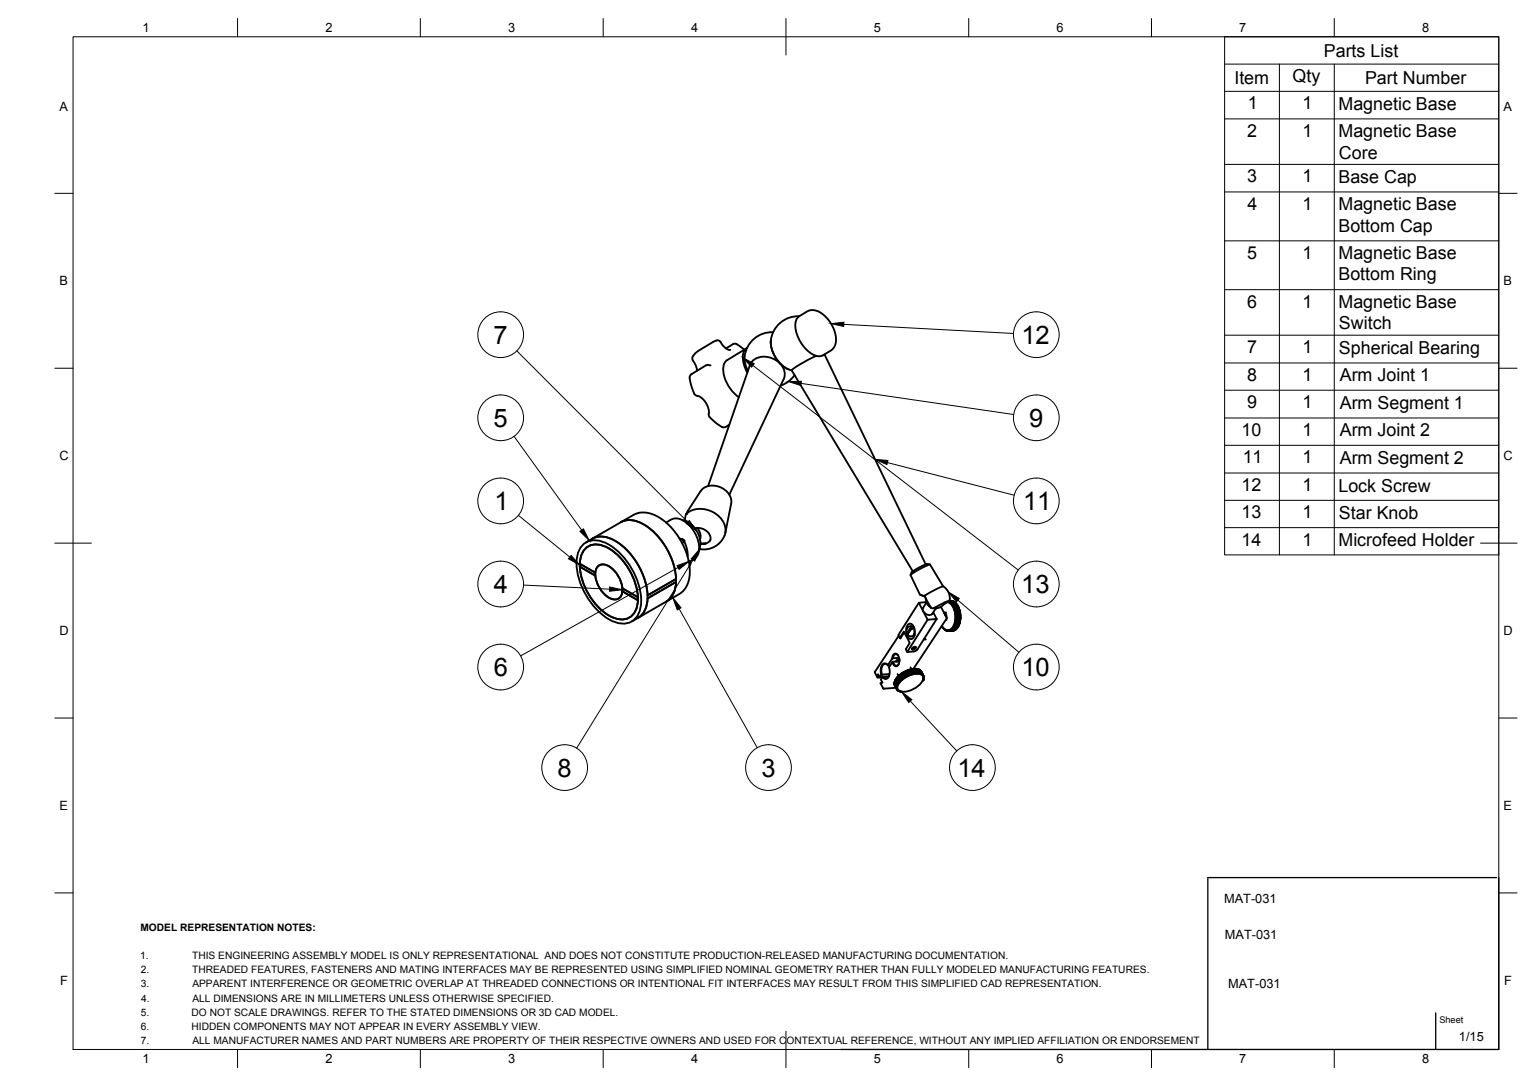
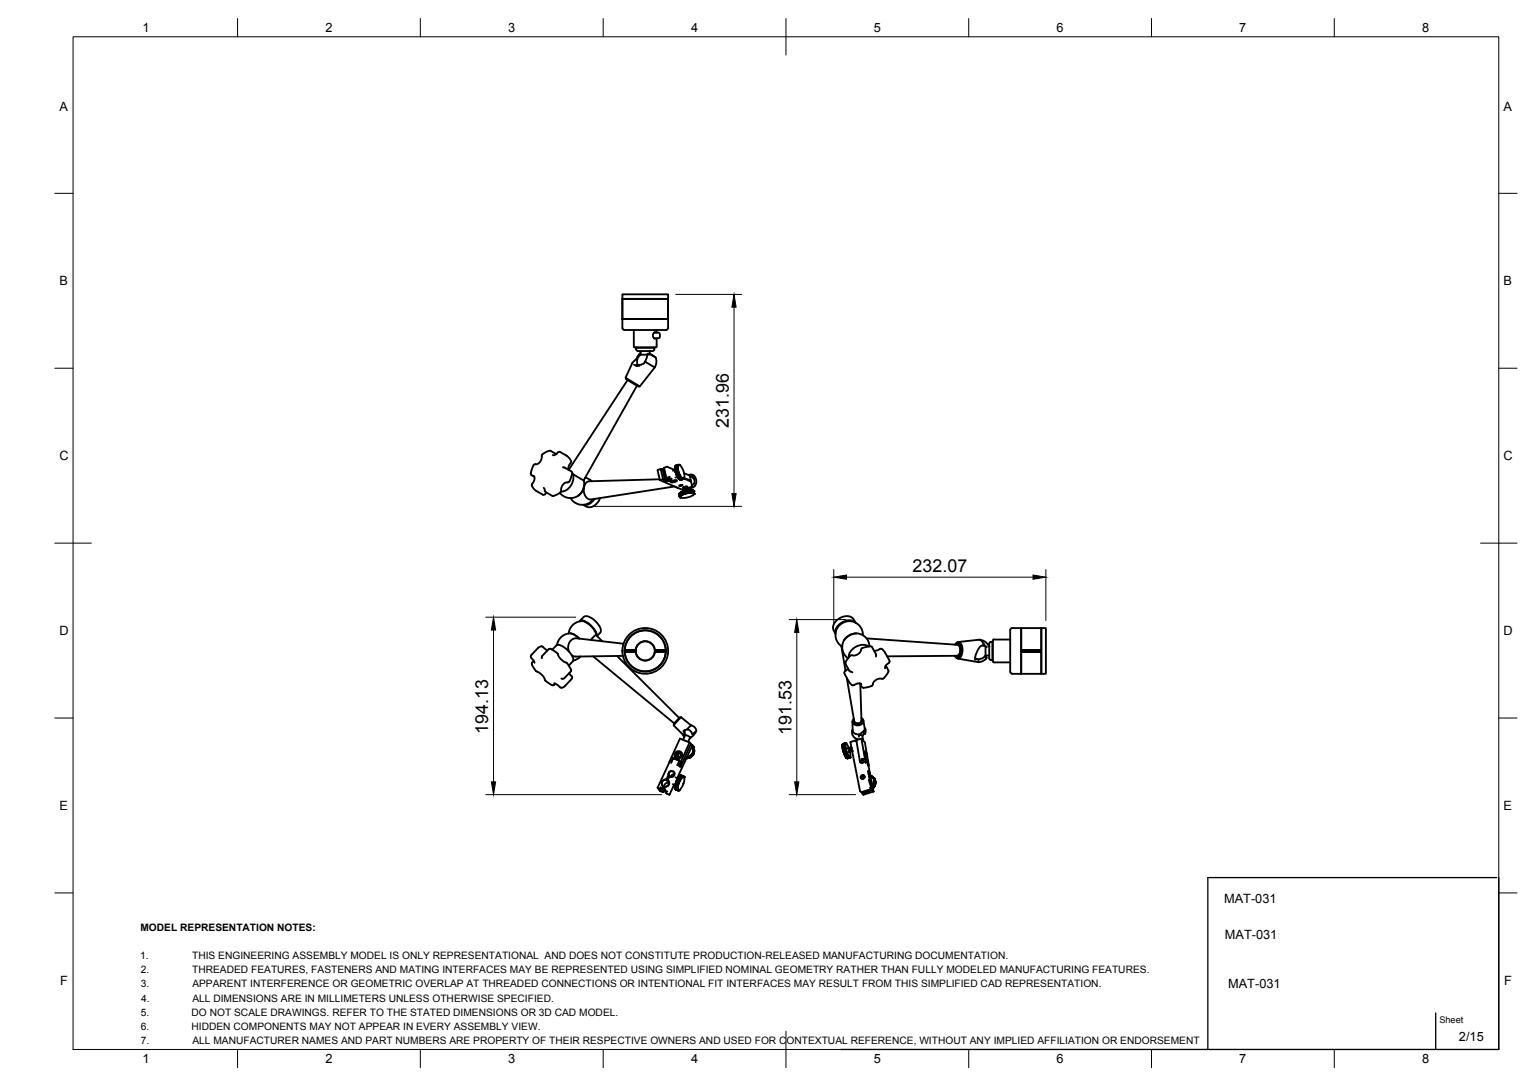
ISO-10303-21;
HEADER;
/* Generated by software containing ST-Developer
 * from STEP Tools, Inc. (www.steptools.com) 
 */

FILE_DESCRIPTION(
/* description */ ('STEP AP214'),
/* implementation_level */ '2;1');

FILE_NAME(
/* name */ 'MAT-031.step',
/* time_stamp */ '2026-11-14T06:58:01-08:00',
/* author */ (''),
/* organization */ (''),
/* preprocessor_version */ 'ST-DEVELOPER v20.2',
/* originating_system */ 'Autodesk Translation Framework v15.17.0.0',
/* authorisation */ '');

FILE_SCHEMA (('AUTOMOTIVE_DESIGN { 1 0 10303 214 3 1 1 }'));
ENDSEC;

DATA;
#10=MECHANICAL_DESIGN_GEOMETRIC_PRESENTATION_REPRESENTATION('',(#1140,#1141,
#1142,#1143,#1144,#1145,#1146,#1147,#1148,#1149,#1150,#1151,#1152,#1153,
#1154,#1155,#1156,#1157,#1158,#1159,#1160,#1161,#1162,#1163,#1164,#1165),
#38635);
#11=ITEM_DEFINED_TRANSFORMATION($,$,#17788,#19729);
#12=ITEM_DEFINED_TRANSFORMATION($,$,#17857,#19730);
#13=ITEM_DEFINED_TRANSFORMATION($,$,#17909,#19731);
#14=ITEM_DEFINED_TRANSFORMATION($,$,#18002,#19732);
#15=ITEM_DEFINED_TRANSFORMATION($,$,#18012,#19733);
#16=ITEM_DEFINED_TRANSFORMATION($,$,#18021,#19734);
#17=ITEM_DEFINED_TRANSFORMATION($,$,#18036,#19735);
#18=ITEM_DEFINED_TRANSFORMATION($,$,#18058,#19736);
#19=ITEM_DEFINED_TRANSFORMATION($,$,#18127,#19737);
#20=ITEM_DEFINED_TRANSFORMATION($,$,#18149,#19738);
#21=ITEM_DEFINED_TRANSFORMATION($,$,#18196,#19739);
#22=ITEM_DEFINED_TRANSFORMATION($,$,#18218,#19740);
#23=ITEM_DEFINED_TRANSFORMATION($,$,#18244,#19741);
#24=ITEM_DEFINED_TRANSFORMATION($,$,#18447,#19742);
#25=(
REPRESENTATION_RELATIONSHIP($,$,#38685,#38684)
REPRESENTATION_RELATIONSHIP_WITH_TRANSFORMATION(#11)
SHAPE_REPRESENTATION_RELATIONSHIP()
);
#26=(
REPRESENTATION_RELATIONSHIP($,$,#38686,#38684)
REPRESENTATION_RELATIONSHIP_WITH_TRANSFORMATION(#12)
SHAPE_REPRESENTATION_RELATIONSHIP()
);
#27=(
REPRESENTATION_RELATIONSHIP($,$,#38687,#38684)
REPRESENTATION_RELATIONSHIP_WITH_TRANSFORMATION(#13)
SHAPE_REPRESENTATION_RELATIONSHIP()
);
#28=(
REPRESENTATION_RELATIONSHIP($,$,#38688,#38684)
REPRESENTATION_RELATIONSHIP_WITH_TRANSFORMATION(#14)
SHAPE_REPRESENTATION_RELATIONSHIP()
);
#29=(
REPRESENTATION_RELATIONSHIP($,$,#38689,#38684)
REPRESENTATION_RELATIONSHIP_WITH_TRANSFORMATION(#15)
SHAPE_REPRESENTATION_RELATIONSHIP()
);
#30=(
REPRESENTATION_RELATIONSHIP($,$,#38690,#38684)
REPRESENTATION_RELATIONSHIP_WITH_TRANSFORMATION(#16)
SHAPE_REPRESENTATION_RELATIONSHIP()
);
#31=(
REPRESENTATION_RELATIONSHIP($,$,#38691,#38684)
REPRESENTATION_RELATIONSHIP_WITH_TRANSFORMATION(#17)
SHAPE_REPRESENTATION_RELATIONSHIP()
);
#32=(
REPRESENTATION_RELATIONSHIP($,$,#38692,#38684)
REPRESENTATION_RELATIONSHIP_WITH_TRANSFORMATION(#18)
SHAPE_REPRESENTATION_RELATIONSHIP()
);
#33=(
REPRESENTATION_RELATIONSHIP($,$,#38693,#38684)
REPRESENTATION_RELATIONSHIP_WITH_TRANSFORMATION(#19)
SHAPE_REPRESENTATION_RELATIONSHIP()
);
#34=(
REPRESENTATION_RELATIONSHIP($,$,#38694,#38684)
REPRESENTATION_RELATIONSHIP_WITH_TRANSFORMATION(#20)
SHAPE_REPRESENTATION_RELATIONSHIP()
);
#35=(
REPRESENTATION_RELATIONSHIP($,$,#38695,#38684)
REPRESENTATION_RELATIONSHIP_WITH_TRANSFORMATION(#21)
SHAPE_REPRESENTATION_RELATIONSHIP()
);
#36=(
REPRESENTATION_RELATIONSHIP($,$,#38696,#38684)
REPRESENTATION_RELATIONSHIP_WITH_TRANSFORMATION(#22)
SHAPE_REPRESENTATION_RELATIONSHIP()
);
#37=(
REPRESENTATION_RELATIONSHIP($,$,#38697,#38684)
REPRESENTATION_RELATIONSHIP_WITH_TRANSFORMATION(#23)
SHAPE_REPRESENTATION_RELATIONSHIP()
);
#38=(
REPRESENTATION_RELATIONSHIP($,$,#38698,#38684)
REPRESENTATION_RELATIONSHIP_WITH_TRANSFORMATION(#24)
SHAPE_REPRESENTATION_RELATIONSHIP()
);
#39=CONTEXT_DEPENDENT_SHAPE_REPRESENTATION(#25,#38670);
#40=CONTEXT_DEPENDENT_SHAPE_REPRESENTATION(#26,#38671);
#41=CONTEXT_DEPENDENT_SHAPE_REPRESENTATION(#27,#38672);
#42=CONTEXT_DEPENDENT_SHAPE_REPRESENTATION(#28,#38673);
#43=CONTEXT_DEPENDENT_SHAPE_REPRESENTATION(#29,#38674);
#44=CONTEXT_DEPENDENT_SHAPE_REPRESENTATION(#30,#38675);
#45=CONTEXT_DEPENDENT_SHAPE_REPRESENTATION(#31,#38676);
#46=CONTEXT_DEPENDENT_SHAPE_REPRESENTATION(#32,#38677);
#47=CONTEXT_DEPENDENT_SHAPE_REPRESENTATION(#33,#38678);
#48=CONTEXT_DEPENDENT_SHAPE_REPRESENTATION(#34,#38679);
#49=CONTEXT_DEPENDENT_SHAPE_REPRESENTATION(#35,#38680);
#50=CONTEXT_DEPENDENT_SHAPE_REPRESENTATION(#36,#38681);
#51=CONTEXT_DEPENDENT_SHAPE_REPRESENTATION(#37,#38682);
#52=CONTEXT_DEPENDENT_SHAPE_REPRESENTATION(#38,#38683);
#53=NEXT_ASSEMBLY_USAGE_OCCURRENCE('Magnetic Base:1','Magnetic Base:1',
'Magnetic Base:1',#38700,#38701,'Magnetic Base:1');
#54=NEXT_ASSEMBLY_USAGE_OCCURRENCE('Magnetic Base Core:1',
'Magnetic Base Core:1','Magnetic Base Core:1',#38700,#38702,
'Magnetic Base Core:1');
#55=NEXT_ASSEMBLY_USAGE_OCCURRENCE('Base Cap:1','Base Cap:1',
'Base Cap:1',#38700,#38703,'Base Cap:1');
#56=NEXT_ASSEMBLY_USAGE_OCCURRENCE('Magnetic Base Bottom Cap:1',
'Magnetic Base Bottom Cap:1','Magnetic Base Bottom Cap:1',#38700,#38704,
'Magnetic Base Bottom Cap:1');
#57=NEXT_ASSEMBLY_USAGE_OCCURRENCE('Magnetic Base Bottom Ring:1',
'Magnetic Base Bottom Ring:1','Magnetic Base Bottom Ring:1',#38700,#38705,
'Magnetic Base Bottom Ring:1');
#58=NEXT_ASSEMBLY_USAGE_OCCURRENCE('Magnetic Base Switch:1',
'Magnetic Base Switch:1','Magnetic Base Switch:1',#38700,#38706,
'Magnetic Base Switch:1');
#59=NEXT_ASSEMBLY_USAGE_OCCURRENCE('Spherical Bearing:1',
'Spherical Bearing:1','Spherical Bearing:1',#38700,#38707,
'Spherical Bearing:1');
#60=NEXT_ASSEMBLY_USAGE_OCCURRENCE('Arm Joint 1:1','Arm Joint 1:1',
'Arm Joint 1:1',#38700,#38708,'Arm Joint 1:1');
#61=NEXT_ASSEMBLY_USAGE_OCCURRENCE('Arm Segment 1:1','Arm Segment 1:1',
'Arm Segment 1:1',#38700,#38709,'Arm Segment 1:1');
#62=NEXT_ASSEMBLY_USAGE_OCCURRENCE('Arm Joint 2:1','Arm Joint 2:1',
'Arm Joint 2:1',#38700,#38710,'Arm Joint 2:1');
#63=NEXT_ASSEMBLY_USAGE_OCCURRENCE('Arm Segment 2:1','Arm Segment 2:1',
'Arm Segment 2:1',#38700,#38711,'Arm Segment 2:1');
#64=NEXT_ASSEMBLY_USAGE_OCCURRENCE('Lock Screw:1','Lock Screw:1',
'Lock Screw:1',#38700,#38712,'Lock Screw:1');
#65=NEXT_ASSEMBLY_USAGE_OCCURRENCE('Star Knob:1','Star Knob:1',
'Star Knob:1',#38700,#38713,'Star Knob:1');
#66=NEXT_ASSEMBLY_USAGE_OCCURRENCE('Microfeed Holder:1',
'Microfeed Holder:1','Microfeed Holder:1',#38700,#38714,
'Microfeed Holder:1');
#67=ELLIPSE('',#18082,0.093043907355238,0.0660721764139862);
#68=ELLIPSE('',#18534,0.424264068711536,0.299999999999714);
#69=ELLIPSE('',#18536,0.424264068712725,0.300000000000503);
#70=ELLIPSE('',#18544,0.424264068711314,0.299999999999553);
#71=ELLIPSE('',#18551,0.424264068712409,0.300000000000364);
#72=ELLIPSE('',#18570,0.424264068711872,0.299999999999922);
#73=ELLIPSE('',#18576,0.42426406871188,0.299999999999951);
#74=ELLIPSE('',#18583,0.424264068709732,0.299999999998459);
#75=ELLIPSE('',#18585,0.424264068710271,0.299999999998872);
#76=ELLIPSE('',#18587,0.424264068711053,0.29999999999941);
#77=ELLIPSE('',#18589,0.424264068710426,0.299999999998988);
#78=SPHERICAL_SURFACE('',#18050,9.);
#79=SPHERICAL_SURFACE('',#18062,1.);
#80=SPHERICAL_SURFACE('',#18074,9.25);
#81=SPHERICAL_SURFACE('',#18083,12.25);
#82=SPHERICAL_SURFACE('',#18107,1.);
#83=SPHERICAL_SURFACE('',#18111,1.);
#84=SPHERICAL_SURFACE('',#18115,1.);
#85=SPHERICAL_SURFACE('',#18118,1.);
#86=SPHERICAL_SURFACE('',#18123,1.);
#87=SPHERICAL_SURFACE('',#18128,15.);
#88=SPHERICAL_SURFACE('',#18136,15.);
#89=SPHERICAL_SURFACE('',#18166,5.5);
#90=SPHERICAL_SURFACE('',#18175,7.70789157434132);
#91=SPHERICAL_SURFACE('',#18197,15.);
#92=SPHERICAL_SURFACE('',#18205,15.);
#93=SPHERICAL_SURFACE('',#18381,2.);
#94=SPHERICAL_SURFACE('',#18383,2.);
#95=SPHERICAL_SURFACE('',#18386,2.);
#96=SPHERICAL_SURFACE('',#18388,2.);
#97=SPHERICAL_SURFACE('',#18394,2.);
#98=SPHERICAL_SURFACE('',#18395,2.);
#99=SPHERICAL_SURFACE('',#18399,2.);
#100=SPHERICAL_SURFACE('',#18400,2.);
#101=SPHERICAL_SURFACE('',#18404,2.);
#102=SPHERICAL_SURFACE('',#18405,2.);
#103=SPHERICAL_SURFACE('',#18409,2.);
#104=SPHERICAL_SURFACE('',#18410,2.);
#105=SPHERICAL_SURFACE('',#18414,2.);
#106=SPHERICAL_SURFACE('',#18416,2.);
#107=SPHERICAL_SURFACE('',#18422,2.);
#108=SPHERICAL_SURFACE('',#18423,2.);
#109=SPHERICAL_SURFACE('',#18424,2.);
#110=SPHERICAL_SURFACE('',#18425,2.);
#111=SPHERICAL_SURFACE('',#18429,2.);
#112=SPHERICAL_SURFACE('',#18431,2.);
#113=SPHERICAL_SURFACE('',#18434,2.);
#114=SPHERICAL_SURFACE('',#18436,2.);
#115=SPHERICAL_SURFACE('',#18442,2.);
#116=SPHERICAL_SURFACE('',#18444,2.);
#117=SPHERICAL_SURFACE('',#18547,0.3);
#118=SPHERICAL_SURFACE('',#18565,0.3);
#119=SPHERICAL_SURFACE('',#18567,0.3);
#120=SPHERICAL_SURFACE('',#18577,0.3);
#121=SPHERICAL_SURFACE('',#18580,0.3);
#122=SPHERICAL_SURFACE('',#18592,0.3);
#123=SPHERICAL_SURFACE('',#18653,5.5);
#124=(
BOUNDED_SURFACE()
B_SPLINE_SURFACE(1,2,((#28370,#28371,#28372,#28373,#28374,#28375,#28376,
#28377,#28378,#28379,#28380,#28381,#28382,#28383,#28384,#28385,#28386,#28387,
#28388,#28389,#28390,#28391,#28392,#28393,#28394,#28395,#28396,#28397,#28398,
#28399,#28400,#28401,#28402,#28403,#28404,#28405,#28406,#28407,#28408,#28409,
#28410,#28411,#28412,#28413,#28414,#28415,#28416,#28417,#28418,#28419,#28420,
#28421,#28422,#28423,#28424,#28425,#28426,#28427,#28428,#28429,#28430,#28431,
#28432,#28433,#28434,#28435,#28436,#28437,#28438,#28439,#28440,#28441,#28442,
#28443,#28444,#28445,#28446,#28447,#28448,#28449,#28450,#28451,#28452,#28453,
#28454,#28455,#28456,#28457,#28458,#28459,#28460,#28461,#28462,#28463,#28464,
#28465,#28466,#28467,#28468,#28469,#28470,#28471,#28472,#28473,#28474,#28475,
#28476,#28477,#28478,#28479,#28480,#28481,#28482,#28483,#28484,#28485,#28486,
#28487,#28488,#28489,#28490,#28491,#28492,#28493,#28494,#28495,#28496,#28497,
#28498,#28499,#28500,#28501,#28502,#28503,#28504,#28505,#28506,#28507,#28508,
#28509,#28510,#28511,#28512,#28513,#28514,#28515,#28516,#28517,#28518,#28519,
#28520,#28521,#28522,#28523,#28524,#28525,#28526,#28527,#28528,#28529,#28530,
#28531,#28532,#28533,#28534,#28535,#28536,#28537,#28538,#28539,#28540,#28541,
#28542,#28543,#28544,#28545,#28546,#28547,#28548,#28549,#28550,#28551,#28552,
#28553,#28554,#28555,#28556,#28557,#28558,#28559,#28560,#28561,#28562,#28563,
#28564,#28565,#28566,#28567,#28568,#28569,#28570,#28571,#28572,#28573,#28574,
#28575,#28576,#28577,#28578,#28579,#28580,#28581,#28582,#28583,#28584,#28585,
#28586,#28587,#28588,#28589,#28590,#28591,#28592,#28593,#28594,#28595,#28596,
#28597,#28598,#28599,#28600,#28601,#28602,#28603,#28604,#28605,#28606,#28607,
#28608,#28609,#28610,#28611,#28612,#28613,#28614,#28615,#28616,#28617,#28618,
#28619,#28620,#28621,#28622,#28623,#28624,#28625,#28626,#28627,#28628,#28629,
#28630,#28631,#28632,#28633,#28634,#28635,#28636,#28637,#28638,#28639,#28640,
#28641,#28642,#28643,#28644,#28645,#28646,#28647,#28648,#28649,#28650,#28651,
#28652,#28653,#28654,#28655,#28656,#28657,#28658,#28659,#28660,#28661,#28662,
#28663,#28664,#28665,#28666,#28667,#28668,#28669,#28670,#28671,#28672,#28673,
#28674,#28675,#28676,#28677,#28678,#28679,#28680,#28681,#28682,#28683,#28684,
#28685,#28686,#28687,#28688,#28689,#28690,#28691,#28692,#28693,#28694,#28695,
#28696,#28697,#28698,#28699,#28700,#28701,#28702,#28703,#28704,#28705,#28706,
#28707,#28708,#28709,#28710,#28711,#28712,#28713,#28714,#28715,#28716,#28717,
#28718,#28719,#28720,#28721,#28722,#28723,#28724,#28725,#28726,#28727,#28728,
#28729,#28730,#28731,#28732,#28733,#28734,#28735,#28736,#28737,#28738,#28739,
#28740,#28741,#28742,#28743,#28744,#28745,#28746,#28747,#28748),(#28749,
#28750,#28751,#28752,#28753,#28754,#28755,#28756,#28757,#28758,#28759,#28760,
#28761,#28762,#28763,#28764,#28765,#28766,#28767,#28768,#28769,#28770,#28771,
#28772,#28773,#28774,#28775,#28776,#28777,#28778,#28779,#28780,#28781,#28782,
#28783,#28784,#28785,#28786,#28787,#28788,#28789,#28790,#28791,#28792,#28793,
#28794,#28795,#28796,#28797,#28798,#28799,#28800,#28801,#28802,#28803,#28804,
#28805,#28806,#28807,#28808,#28809,#28810,#28811,#28812,#28813,#28814,#28815,
#28816,#28817,#28818,#28819,#28820,#28821,#28822,#28823,#28824,#28825,#28826,
#28827,#28828,#28829,#28830,#28831,#28832,#28833,#28834,#28835,#28836,#28837,
#28838,#28839,#28840,#28841,#28842,#28843,#28844,#28845,#28846,#28847,#28848,
#28849,#28850,#28851,#28852,#28853,#28854,#28855,#28856,#28857,#28858,#28859,
#28860,#28861,#28862,#28863,#28864,#28865,#28866,#28867,#28868,#28869,#28870,
#28871,#28872,#28873,#28874,#28875,#28876,#28877,#28878,#28879,#28880,#28881,
#28882,#28883,#28884,#28885,#28886,#28887,#28888,#28889,#28890,#28891,#28892,
#28893,#28894,#28895,#28896,#28897,#28898,#28899,#28900,#28901,#28902,#28903,
#28904,#28905,#28906,#28907,#28908,#28909,#28910,#28911,#28912,#28913,#28914,
#28915,#28916,#28917,#28918,#28919,#28920,#28921,#28922,#28923,#28924,#28925,
#28926,#28927,#28928,#28929,#28930,#28931,#28932,#28933,#28934,#28935,#28936,
#28937,#28938,#28939,#28940,#28941,#28942,#28943,#28944,#28945,#28946,#28947,
#28948,#28949,#28950,#28951,#28952,#28953,#28954,#28955,#28956,#28957,#28958,
#28959,#28960,#28961,#28962,#28963,#28964,#28965,#28966,#28967,#28968,#28969,
#28970,#28971,#28972,#28973,#28974,#28975,#28976,#28977,#28978,#28979,#28980,
#28981,#28982,#28983,#28984,#28985,#28986,#28987,#28988,#28989,#28990,#28991,
#28992,#28993,#28994,#28995,#28996,#28997,#28998,#28999,#29000,#29001,#29002,
#29003,#29004,#29005,#29006,#29007,#29008,#29009,#29010,#29011,#29012,#29013,
#29014,#29015,#29016,#29017,#29018,#29019,#29020,#29021,#29022,#29023,#29024,
#29025,#29026,#29027,#29028,#29029,#29030,#29031,#29032,#29033,#29034,#29035,
#29036,#29037,#29038,#29039,#29040,#29041,#29042,#29043,#29044,#29045,#29046,
#29047,#29048,#29049,#29050,#29051,#29052,#29053,#29054,#29055,#29056,#29057,
#29058,#29059,#29060,#29061,#29062,#29063,#29064,#29065,#29066,#29067,#29068,
#29069,#29070,#29071,#29072,#29073,#29074,#29075,#29076,#29077,#29078,#29079,
#29080,#29081,#29082,#29083,#29084,#29085,#29086,#29087,#29088,#29089,#29090,
#29091,#29092,#29093,#29094,#29095,#29096,#29097,#29098,#29099,#29100,#29101,
#29102,#29103,#29104,#29105,#29106,#29107,#29108,#29109,#29110,#29111,#29112,
#29113,#29114,#29115,#29116,#29117,#29118,#29119,#29120,#29121,#29122,#29123,
#29124,#29125,#29126,#29127)),.UNSPECIFIED.,.F.,.F.,.F.)
B_SPLINE_SURFACE_WITH_KNOTS((2,2),(3,2,2,2,2,2,2,2,2,2,2,2,2,2,2,2,2,2,
2,2,2,2,2,2,2,2,2,2,2,2,2,2,2,2,2,2,2,2,2,2,2,2,2,2,2,2,2,2,2,2,2,2,2,2,
2,2,2,2,2,2,2,2,2,2,2,2,2,2,2,2,2,2,2,2,2,2,2,2,2,2,2,2,2,2,2,2,2,2,2,2,
2,2,2,2,2,2,2,2,2,2,2,2,2,2,2,2,2,2,2,2,2,2,2,2,2,2,2,2,2,2,2,2,2,2,2,2,
2,2,2,2,2,2,2,2,2,2,2,2,2,2,2,2,2,2,2,2,2,2,2,2,2,2,2,2,2,2,2,2,2,2,2,2,
2,2,2,2,2,2,2,2,2,2,2,2,2,2,2,2,2,2,2,2,2,2,2,2,2,2,2,3),(0.,1.),(0.,0.00520833333333333,
0.0104166666666667,0.015625,0.0208333333333333,0.0260416666666667,0.03125,
0.0364583333333333,0.0416666666666667,0.046875,0.0520833333333333,0.0572916666666667,
0.0625,0.0677083333333333,0.0729166666666667,0.078125,0.0833333333333333,
0.0885416666666667,0.09375,0.0989583333333333,0.104166666666667,0.109375,
0.114583333333333,0.119791666666667,0.125,0.130208333333333,0.135416666666667,
0.140625,0.145833333333333,0.151041666666667,0.15625,0.161458333333333,
0.166666666666667,0.171875,0.177083333333333,0.182291666666667,0.1875,0.192708333333333,
0.197916666666667,0.203125,0.208333333333333,0.213541666666667,0.21875,
0.223958333333333,0.229166666666667,0.234375,0.239583333333333,0.244791666666667,
0.25,0.255208333333333,0.260416666666667,0.265625,0.270833333333333,0.276041666666667,
0.28125,0.286458333333333,0.291666666666667,0.296875,0.302083333333333,
0.307291666666667,0.3125,0.317708333333333,0.322916666666667,0.328125,0.333333333333333,
0.338541666666667,0.34375,0.348958333333333,0.354166666666667,0.359375,
0.364583333333333,0.369791666666667,0.375,0.380208333333333,0.385416666666667,
0.390625,0.395833333333333,0.401041666666667,0.40625,0.411458333333333,
0.416666666666667,0.421875,0.427083333333333,0.432291666666667,0.4375,0.442708333333333,
0.447916666666667,0.453125,0.458333333333333,0.463541666666667,0.46875,
0.473958333333333,0.479166666666667,0.484375,0.489583333333333,0.494791666666667,
0.5,0.505208333333333,0.510416666666667,0.515625,0.520833333333333,0.526041666666667,
0.53125,0.536458333333333,0.541666666666667,0.546875,0.552083333333333,
0.557291666666667,0.5625,0.567708333333333,0.572916666666667,0.578125,0.583333333333333,
0.588541666666667,0.59375,0.598958333333333,0.604166666666667,0.609375,
0.614583333333333,0.619791666666667,0.625,0.630208333333333,0.635416666666667,
0.640625,0.645833333333333,0.651041666666667,0.65625,0.661458333333333,
0.666666666666667,0.671875,0.677083333333333,0.682291666666667,0.6875,0.692708333333333,
0.697916666666667,0.703125,0.708333333333333,0.713541666666667,0.71875,
0.723958333333333,0.729166666666667,0.734375,0.739583333333333,0.744791666666667,
0.75,0.755208333333333,0.760416666666667,0.765625,0.770833333333333,0.776041666666667,
0.78125,0.786458333333333,0.791666666666667,0.796875,0.802083333333333,
0.807291666666667,0.8125,0.817708333333333,0.822916666666667,0.828125,0.833333333333333,
0.838541666666667,0.84375,0.848958333333333,0.854166666666667,0.859375,
0.864583333333333,0.869791666666667,0.875,0.880208333333333,0.885416666666667,
0.890625,0.895833333333333,0.901041666666667,0.90625,0.911458333333333,
0.916666666666667,0.921875,0.927083333333333,0.932291666666667,0.9375,0.942708333333333,
0.947916666666667,0.953125,0.958333333333333,0.963541666666667,0.96875,
0.973958333333333,0.979166666666667,0.984246579235552),.UNSPECIFIED.)
GEOMETRIC_REPRESENTATION_ITEM()
RATIONAL_B_SPLINE_SURFACE(((1.,0.866025403784439,1.,0.866025403784439,1.,
0.866025403784439,1.,0.866025403784439,1.,0.866025403784439,1.,0.866025403784439,
1.,0.866025403784439,1.,0.866025403784439,1.,0.866025403784439,1.,0.866025403784439,
1.,0.866025403784439,1.,0.866025403784439,1.,0.866025403784439,1.,0.866025403784439,
1.,0.866025403784439,1.,0.866025403784439,1.,0.866025403784439,1.,0.866025403784439,
1.,0.866025403784439,1.,0.866025403784439,1.,0.866025403784439,1.,0.866025403784439,
1.,0.866025403784439,1.,0.866025403784439,1.,0.866025403784439,1.,0.866025403784439,
1.,0.866025403784439,1.,0.866025403784439,1.,0.866025403784439,1.,0.866025403784439,
1.,0.866025403784439,1.,0.866025403784439,1.,0.866025403784439,1.,0.866025403784439,
1.,0.866025403784439,1.,0.866025403784439,1.,0.866025403784439,1.,0.866025403784439,
1.,0.866025403784439,1.,0.866025403784439,1.,0.866025403784439,1.,0.866025403784439,
1.,0.866025403784439,1.,0.866025403784439,1.,0.866025403784439,1.,0.866025403784439,
1.,0.866025403784439,1.,0.866025403784439,1.,0.866025403784439,1.,0.866025403784439,
1.,0.866025403784439,1.,0.866025403784439,1.,0.866025403784439,1.,0.866025403784439,
1.,0.866025403784439,1.,0.866025403784439,1.,0.866025403784439,1.,0.866025403784439,
1.,0.866025403784439,1.,0.866025403784439,1.,0.866025403784439,1.,0.866025403784439,
1.,0.866025403784439,1.,0.866025403784439,1.,0.866025403784439,1.,0.866025403784439,
1.,0.866025403784439,1.,0.866025403784439,1.,0.866025403784439,1.,0.866025403784439,
1.,0.866025403784439,1.,0.866025403784439,1.,0.866025403784439,1.,0.866025403784439,
1.,0.866025403784439,1.,0.866025403784439,1.,0.866025403784439,1.,0.866025403784439,
1.,0.866025403784439,1.,0.866025403784439,1.,0.866025403784439,1.,0.866025403784439,
1.,0.866025403784439,1.,0.866025403784439,1.,0.866025403784439,1.,0.866025403784439,
1.,0.866025403784439,1.,0.866025403784439,1.,0.866025403784439,1.,0.866025403784439,
1.,0.866025403784439,1.,0.866025403784439,1.,0.866025403784439,1.,0.866025403784439,
1.,0.866025403784439,1.,0.866025403784439,1.,0.866025403784439,1.,0.866025403784439,
1.,0.866025403784439,1.,0.866025403784439,1.,0.866025403784439,1.,0.866025403784439,
1.,0.866025403784439,1.,0.866025403784439,1.,0.866025403784439,1.,0.866025403784439,
1.,0.866025403784439,1.,0.866025403784439,1.,0.866025403784439,1.,0.866025403784439,
1.,0.866025403784439,1.,0.866025403784439,1.,0.866025403784439,1.,0.866025403784439,
1.,0.866025403784439,1.,0.866025403784439,1.,0.866025403784439,1.,0.866025403784439,
1.,0.866025403784439,1.,0.866025403784439,1.,0.866025403784439,1.,0.866025403784439,
1.,0.866025403784439,1.,0.866025403784439,1.,0.866025403784439,1.,0.866025403784439,
1.,0.866025403784439,1.,0.866025403784439,1.,0.866025403784439,1.,0.866025403784439,
1.,0.866025403784439,1.,0.866025403784439,1.,0.866025403784439,1.,0.866025403784439,
1.,0.866025403784439,1.,0.866025403784439,1.,0.866025403784439,1.,0.866025403784439,
1.,0.866025403784439,1.,0.866025403784439,1.,0.866025403784439,1.,0.866025403784439,
1.,0.866025403784439,1.,0.866025403784439,1.,0.866025403784439,1.,0.866025403784439,
1.,0.866025403784439,1.,0.866025403784439,1.,0.866025403784439,1.,0.866025403784439,
1.,0.866025403784439,1.,0.866025403784439,1.,0.866025403784439,1.,0.866025403784439,
1.,0.866025403784439,1.,0.866025403784439,1.,0.866025403784439,1.,0.866025403784439,
1.,0.866025403784439,1.,0.866025403784439,1.,0.866025403784439,1.,0.866025403784439,
1.,0.866025403784439,1.,0.866025403784439,1.,0.866025403784439,1.,0.866025403784439,
1.,0.866025403784439,1.,0.866025403784439,1.,0.866025403784439,1.,0.866025403784439,
1.,0.866025403784439,1.,0.866025403784439,1.,0.866025403784439,1.,0.866025403784439,
1.,0.866025403784439,1.,0.866025403784439,1.,0.866025403784439,1.,0.866025403784439,
1.,0.866025403784439,1.,0.866025403784439,1.,0.866025403784439,1.,0.866025403784439,
1.,0.866025403784439,1.,0.866025403784439,1.,0.866025403784439,1.,0.866025403784439,
1.,0.866025403784439,1.,0.866025403784439,1.,0.869328786836457,0.993556135519056),
(1.,0.866025403784439,1.,0.866025403784439,1.,0.866025403784439,1.,0.866025403784439,
1.,0.866025403784439,1.,0.866025403784439,1.,0.866025403784439,1.,0.866025403784439,
1.,0.866025403784439,1.,0.866025403784439,1.,0.866025403784439,1.,0.866025403784439,
1.,0.866025403784439,1.,0.866025403784439,1.,0.866025403784439,1.,0.866025403784439,
1.,0.866025403784439,1.,0.866025403784439,1.,0.866025403784439,1.,0.866025403784439,
1.,0.866025403784439,1.,0.866025403784439,1.,0.866025403784439,1.,0.866025403784439,
1.,0.866025403784439,1.,0.866025403784439,1.,0.866025403784439,1.,0.866025403784439,
1.,0.866025403784439,1.,0.866025403784439,1.,0.866025403784439,1.,0.866025403784439,
1.,0.866025403784439,1.,0.866025403784439,1.,0.866025403784439,1.,0.866025403784439,
1.,0.866025403784439,1.,0.866025403784439,1.,0.866025403784439,1.,0.866025403784439,
1.,0.866025403784439,1.,0.866025403784439,1.,0.866025403784439,1.,0.866025403784439,
1.,0.866025403784439,1.,0.866025403784439,1.,0.866025403784439,1.,0.866025403784439,
1.,0.866025403784439,1.,0.866025403784439,1.,0.866025403784439,1.,0.866025403784439,
1.,0.866025403784439,1.,0.866025403784439,1.,0.866025403784439,1.,0.866025403784439,
1.,0.866025403784439,1.,0.866025403784439,1.,0.866025403784439,1.,0.866025403784439,
1.,0.866025403784439,1.,0.866025403784439,1.,0.866025403784439,1.,0.866025403784439,
1.,0.866025403784439,1.,0.866025403784439,1.,0.866025403784439,1.,0.866025403784439,
1.,0.866025403784439,1.,0.866025403784439,1.,0.866025403784439,1.,0.866025403784439,
1.,0.866025403784439,1.,0.866025403784439,1.,0.866025403784439,1.,0.866025403784439,
1.,0.866025403784439,1.,0.866025403784439,1.,0.866025403784439,1.,0.866025403784439,
1.,0.866025403784439,1.,0.866025403784439,1.,0.866025403784439,1.,0.866025403784439,
1.,0.866025403784439,1.,0.866025403784439,1.,0.866025403784439,1.,0.866025403784439,
1.,0.866025403784439,1.,0.866025403784439,1.,0.866025403784439,1.,0.866025403784439,
1.,0.866025403784439,1.,0.866025403784439,1.,0.866025403784439,1.,0.866025403784439,
1.,0.866025403784439,1.,0.866025403784439,1.,0.866025403784439,1.,0.866025403784439,
1.,0.866025403784439,1.,0.866025403784439,1.,0.866025403784439,1.,0.866025403784439,
1.,0.866025403784439,1.,0.866025403784439,1.,0.866025403784439,1.,0.866025403784439,
1.,0.866025403784439,1.,0.866025403784439,1.,0.866025403784439,1.,0.866025403784439,
1.,0.866025403784439,1.,0.866025403784439,1.,0.866025403784439,1.,0.866025403784439,
1.,0.866025403784439,1.,0.866025403784439,1.,0.866025403784439,1.,0.866025403784439,
1.,0.866025403784439,1.,0.866025403784439,1.,0.866025403784439,1.,0.866025403784439,
1.,0.866025403784439,1.,0.866025403784439,1.,0.866025403784439,1.,0.866025403784439,
1.,0.866025403784439,1.,0.866025403784439,1.,0.866025403784439,1.,0.866025403784439,
1.,0.866025403784439,1.,0.866025403784439,1.,0.866025403784439,1.,0.866025403784439,
1.,0.866025403784439,1.,0.866025403784439,1.,0.866025403784439,1.,0.866025403784439,
1.,0.866025403784439,1.,0.866025403784439,1.,0.866025403784439,1.,0.866025403784439,
1.,0.866025403784439,1.,0.866025403784439,1.,0.866025403784439,1.,0.866025403784439,
1.,0.866025403784439,1.,0.866025403784439,1.,0.866025403784439,1.,0.866025403784439,
1.,0.866025403784439,1.,0.866025403784439,1.,0.866025403784439,1.,0.866025403784439,
1.,0.866025403784439,1.,0.866025403784439,1.,0.866025403784439,1.,0.866025403784439,
1.,0.866025403784439,1.,0.866025403784439,1.,0.866025403784439,1.,0.866025403784439,
1.,0.866025403784439,1.,0.866025403784439,1.,0.866025403784439,1.,0.866025403784439,
1.,0.866025403784439,1.,0.866025403784439,1.,0.866025403784439,1.,0.866025403784439,
1.,0.866025403784439,1.,0.866025403784439,1.,0.866025403784439,1.,0.866025403784439,
1.,0.866025403784439,1.,0.866025403784439,1.,0.866025403784439,1.,0.866025403784439,
1.,0.866025403784439,1.,0.866025403784439,1.,0.866025403784439,1.,0.866025403784439,
1.,0.866025403784439,1.,0.866025403784439,1.,0.866025403784439,1.,0.866025403784439,
1.,0.869328786836457,0.993556135519056)))
REPRESENTATION_ITEM('')
SURFACE()
);
#125=(
BOUNDED_SURFACE()
B_SPLINE_SURFACE(1,2,((#29128,#29129,#29130,#29131,#29132,#29133,#29134,
#29135,#29136,#29137,#29138,#29139,#29140,#29141,#29142,#29143,#29144,#29145,
#29146,#29147,#29148,#29149,#29150,#29151,#29152,#29153,#29154,#29155,#29156,
#29157,#29158,#29159,#29160,#29161,#29162,#29163,#29164,#29165,#29166,#29167,
#29168,#29169,#29170,#29171,#29172,#29173,#29174,#29175,#29176,#29177,#29178,
#29179,#29180,#29181,#29182,#29183,#29184,#29185,#29186,#29187,#29188,#29189,
#29190,#29191,#29192,#29193,#29194,#29195,#29196,#29197,#29198,#29199,#29200,
#29201,#29202,#29203,#29204,#29205,#29206,#29207,#29208,#29209,#29210,#29211,
#29212,#29213,#29214,#29215,#29216,#29217,#29218,#29219,#29220,#29221,#29222,
#29223,#29224,#29225,#29226,#29227,#29228,#29229,#29230,#29231,#29232,#29233,
#29234,#29235,#29236,#29237,#29238,#29239,#29240,#29241,#29242,#29243,#29244,
#29245,#29246,#29247,#29248,#29249,#29250,#29251,#29252,#29253,#29254,#29255,
#29256,#29257,#29258,#29259,#29260,#29261,#29262,#29263,#29264,#29265,#29266,
#29267,#29268,#29269,#29270,#29271,#29272,#29273,#29274,#29275,#29276,#29277,
#29278,#29279,#29280,#29281,#29282,#29283,#29284,#29285,#29286,#29287,#29288,
#29289,#29290,#29291,#29292,#29293,#29294,#29295,#29296,#29297,#29298,#29299,
#29300,#29301,#29302,#29303,#29304,#29305,#29306,#29307,#29308,#29309,#29310,
#29311,#29312,#29313,#29314,#29315,#29316,#29317,#29318,#29319,#29320,#29321,
#29322,#29323,#29324,#29325,#29326,#29327,#29328,#29329,#29330,#29331,#29332,
#29333,#29334,#29335,#29336,#29337,#29338,#29339,#29340,#29341,#29342,#29343,
#29344,#29345,#29346,#29347,#29348,#29349,#29350,#29351,#29352,#29353,#29354,
#29355,#29356,#29357,#29358,#29359,#29360,#29361,#29362,#29363,#29364,#29365,
#29366,#29367,#29368,#29369,#29370,#29371,#29372,#29373,#29374,#29375,#29376,
#29377,#29378,#29379,#29380,#29381,#29382,#29383,#29384,#29385,#29386,#29387,
#29388,#29389,#29390,#29391,#29392,#29393,#29394,#29395,#29396,#29397,#29398,
#29399,#29400,#29401,#29402,#29403,#29404,#29405,#29406,#29407,#29408,#29409,
#29410,#29411,#29412,#29413,#29414,#29415,#29416,#29417,#29418,#29419,#29420,
#29421,#29422,#29423,#29424,#29425,#29426,#29427,#29428,#29429,#29430,#29431,
#29432,#29433,#29434,#29435,#29436,#29437,#29438,#29439,#29440,#29441,#29442,
#29443,#29444,#29445,#29446,#29447,#29448,#29449,#29450,#29451,#29452,#29453,
#29454,#29455,#29456,#29457,#29458,#29459,#29460,#29461,#29462,#29463,#29464,
#29465,#29466,#29467,#29468,#29469,#29470,#29471,#29472,#29473,#29474,#29475,
#29476,#29477,#29478,#29479,#29480,#29481,#29482,#29483,#29484,#29485,#29486,
#29487,#29488,#29489,#29490,#29491,#29492,#29493,#29494,#29495,#29496,#29497,
#29498,#29499,#29500,#29501,#29502,#29503,#29504,#29505,#29506),(#29507,
#29508,#29509,#29510,#29511,#29512,#29513,#29514,#29515,#29516,#29517,#29518,
#29519,#29520,#29521,#29522,#29523,#29524,#29525,#29526,#29527,#29528,#29529,
#29530,#29531,#29532,#29533,#29534,#29535,#29536,#29537,#29538,#29539,#29540,
#29541,#29542,#29543,#29544,#29545,#29546,#29547,#29548,#29549,#29550,#29551,
#29552,#29553,#29554,#29555,#29556,#29557,#29558,#29559,#29560,#29561,#29562,
#29563,#29564,#29565,#29566,#29567,#29568,#29569,#29570,#29571,#29572,#29573,
#29574,#29575,#29576,#29577,#29578,#29579,#29580,#29581,#29582,#29583,#29584,
#29585,#29586,#29587,#29588,#29589,#29590,#29591,#29592,#29593,#29594,#29595,
#29596,#29597,#29598,#29599,#29600,#29601,#29602,#29603,#29604,#29605,#29606,
#29607,#29608,#29609,#29610,#29611,#29612,#29613,#29614,#29615,#29616,#29617,
#29618,#29619,#29620,#29621,#29622,#29623,#29624,#29625,#29626,#29627,#29628,
#29629,#29630,#29631,#29632,#29633,#29634,#29635,#29636,#29637,#29638,#29639,
#29640,#29641,#29642,#29643,#29644,#29645,#29646,#29647,#29648,#29649,#29650,
#29651,#29652,#29653,#29654,#29655,#29656,#29657,#29658,#29659,#29660,#29661,
#29662,#29663,#29664,#29665,#29666,#29667,#29668,#29669,#29670,#29671,#29672,
#29673,#29674,#29675,#29676,#29677,#29678,#29679,#29680,#29681,#29682,#29683,
#29684,#29685,#29686,#29687,#29688,#29689,#29690,#29691,#29692,#29693,#29694,
#29695,#29696,#29697,#29698,#29699,#29700,#29701,#29702,#29703,#29704,#29705,
#29706,#29707,#29708,#29709,#29710,#29711,#29712,#29713,#29714,#29715,#29716,
#29717,#29718,#29719,#29720,#29721,#29722,#29723,#29724,#29725,#29726,#29727,
#29728,#29729,#29730,#29731,#29732,#29733,#29734,#29735,#29736,#29737,#29738,
#29739,#29740,#29741,#29742,#29743,#29744,#29745,#29746,#29747,#29748,#29749,
#29750,#29751,#29752,#29753,#29754,#29755,#29756,#29757,#29758,#29759,#29760,
#29761,#29762,#29763,#29764,#29765,#29766,#29767,#29768,#29769,#29770,#29771,
#29772,#29773,#29774,#29775,#29776,#29777,#29778,#29779,#29780,#29781,#29782,
#29783,#29784,#29785,#29786,#29787,#29788,#29789,#29790,#29791,#29792,#29793,
#29794,#29795,#29796,#29797,#29798,#29799,#29800,#29801,#29802,#29803,#29804,
#29805,#29806,#29807,#29808,#29809,#29810,#29811,#29812,#29813,#29814,#29815,
#29816,#29817,#29818,#29819,#29820,#29821,#29822,#29823,#29824,#29825,#29826,
#29827,#29828,#29829,#29830,#29831,#29832,#29833,#29834,#29835,#29836,#29837,
#29838,#29839,#29840,#29841,#29842,#29843,#29844,#29845,#29846,#29847,#29848,
#29849,#29850,#29851,#29852,#29853,#29854,#29855,#29856,#29857,#29858,#29859,
#29860,#29861,#29862,#29863,#29864,#29865,#29866,#29867,#29868,#29869,#29870,
#29871,#29872,#29873,#29874,#29875,#29876,#29877,#29878,#29879,#29880,#29881,
#29882,#29883,#29884,#29885)),.UNSPECIFIED.,.F.,.F.,.F.)
B_SPLINE_SURFACE_WITH_KNOTS((2,2),(3,2,2,2,2,2,2,2,2,2,2,2,2,2,2,2,2,2,
2,2,2,2,2,2,2,2,2,2,2,2,2,2,2,2,2,2,2,2,2,2,2,2,2,2,2,2,2,2,2,2,2,2,2,2,
2,2,2,2,2,2,2,2,2,2,2,2,2,2,2,2,2,2,2,2,2,2,2,2,2,2,2,2,2,2,2,2,2,2,2,2,
2,2,2,2,2,2,2,2,2,2,2,2,2,2,2,2,2,2,2,2,2,2,2,2,2,2,2,2,2,2,2,2,2,2,2,2,
2,2,2,2,2,2,2,2,2,2,2,2,2,2,2,2,2,2,2,2,2,2,2,2,2,2,2,2,2,2,2,2,2,2,2,2,
2,2,2,2,2,2,2,2,2,2,2,2,2,2,2,2,2,2,2,2,2,2,2,2,2,2,2,3),(0.,1.),(0.,0.00520833333333333,
0.0104166666666667,0.015625,0.0208333333333333,0.0260416666666667,0.03125,
0.0364583333333333,0.0416666666666667,0.046875,0.0520833333333333,0.0572916666666667,
0.0625,0.0677083333333333,0.0729166666666667,0.078125,0.0833333333333333,
0.0885416666666667,0.09375,0.0989583333333333,0.104166666666667,0.109375,
0.114583333333333,0.119791666666667,0.125,0.130208333333333,0.135416666666667,
0.140625,0.145833333333333,0.151041666666667,0.15625,0.161458333333333,
0.166666666666667,0.171875,0.177083333333333,0.182291666666667,0.1875,0.192708333333333,
0.197916666666667,0.203125,0.208333333333333,0.213541666666667,0.21875,
0.223958333333333,0.229166666666667,0.234375,0.239583333333333,0.244791666666667,
0.25,0.255208333333333,0.260416666666667,0.265625,0.270833333333333,0.276041666666667,
0.28125,0.286458333333333,0.291666666666667,0.296875,0.302083333333333,
0.307291666666667,0.3125,0.317708333333333,0.322916666666667,0.328125,0.333333333333333,
0.338541666666667,0.34375,0.348958333333333,0.354166666666667,0.359375,
0.364583333333333,0.369791666666667,0.375,0.380208333333333,0.385416666666667,
0.390625,0.395833333333333,0.401041666666667,0.40625,0.411458333333333,
0.416666666666667,0.421875,0.427083333333333,0.432291666666667,0.4375,0.442708333333333,
0.447916666666667,0.453125,0.458333333333333,0.463541666666667,0.46875,
0.473958333333333,0.479166666666667,0.484375,0.489583333333333,0.494791666666667,
0.5,0.505208333333333,0.510416666666667,0.515625,0.520833333333333,0.526041666666667,
0.53125,0.536458333333333,0.541666666666667,0.546875,0.552083333333333,
0.557291666666667,0.5625,0.567708333333333,0.572916666666667,0.578125,0.583333333333333,
0.588541666666667,0.59375,0.598958333333333,0.604166666666667,0.609375,
0.614583333333333,0.619791666666667,0.625,0.630208333333333,0.635416666666667,
0.640625,0.645833333333333,0.651041666666667,0.65625,0.661458333333333,
0.666666666666667,0.671875,0.677083333333333,0.682291666666667,0.6875,0.692708333333333,
0.697916666666667,0.703125,0.708333333333333,0.713541666666667,0.71875,
0.723958333333333,0.729166666666667,0.734375,0.739583333333333,0.744791666666667,
0.75,0.755208333333333,0.760416666666667,0.765625,0.770833333333333,0.776041666666667,
0.78125,0.786458333333333,0.791666666666667,0.796875,0.802083333333333,
0.807291666666667,0.8125,0.817708333333333,0.822916666666667,0.828125,0.833333333333333,
0.838541666666667,0.84375,0.848958333333333,0.854166666666667,0.859375,
0.864583333333333,0.869791666666667,0.875,0.880208333333333,0.885416666666667,
0.890625,0.895833333333333,0.901041666666667,0.90625,0.911458333333333,
0.916666666666667,0.921875,0.927083333333333,0.932291666666667,0.9375,0.942708333333333,
0.947916666666667,0.953125,0.958333333333333,0.963541666666667,0.96875,
0.973958333333333,0.979166666666667,0.984246579355594),.UNSPECIFIED.)
GEOMETRIC_REPRESENTATION_ITEM()
RATIONAL_B_SPLINE_SURFACE(((1.,0.866025403784439,1.,0.866025403784439,1.,
0.866025403784439,1.,0.866025403784439,1.,0.866025403784439,1.,0.866025403784439,
1.,0.866025403784439,1.,0.866025403784439,1.,0.866025403784439,1.,0.866025403784439,
1.,0.866025403784439,1.,0.866025403784439,1.,0.866025403784439,1.,0.866025403784439,
1.,0.866025403784439,1.,0.866025403784439,1.,0.866025403784439,1.,0.866025403784439,
1.,0.866025403784439,1.,0.866025403784439,1.,0.866025403784439,1.,0.866025403784439,
1.,0.866025403784439,1.,0.866025403784439,1.,0.866025403784439,1.,0.866025403784439,
1.,0.866025403784439,1.,0.866025403784439,1.,0.866025403784439,1.,0.866025403784439,
1.,0.866025403784439,1.,0.866025403784439,1.,0.866025403784439,1.,0.866025403784439,
1.,0.866025403784439,1.,0.866025403784439,1.,0.866025403784439,1.,0.866025403784439,
1.,0.866025403784439,1.,0.866025403784439,1.,0.866025403784439,1.,0.866025403784439,
1.,0.866025403784439,1.,0.866025403784439,1.,0.866025403784439,1.,0.866025403784439,
1.,0.866025403784439,1.,0.866025403784439,1.,0.866025403784439,1.,0.866025403784439,
1.,0.866025403784439,1.,0.866025403784439,1.,0.866025403784439,1.,0.866025403784439,
1.,0.866025403784439,1.,0.866025403784439,1.,0.866025403784439,1.,0.866025403784439,
1.,0.866025403784439,1.,0.866025403784439,1.,0.866025403784439,1.,0.866025403784439,
1.,0.866025403784439,1.,0.866025403784439,1.,0.866025403784439,1.,0.866025403784439,
1.,0.866025403784439,1.,0.866025403784439,1.,0.866025403784439,1.,0.866025403784439,
1.,0.866025403784439,1.,0.866025403784439,1.,0.866025403784439,1.,0.866025403784439,
1.,0.866025403784439,1.,0.866025403784439,1.,0.866025403784439,1.,0.866025403784439,
1.,0.866025403784439,1.,0.866025403784439,1.,0.866025403784439,1.,0.866025403784439,
1.,0.866025403784439,1.,0.866025403784439,1.,0.866025403784439,1.,0.866025403784439,
1.,0.866025403784439,1.,0.866025403784439,1.,0.866025403784439,1.,0.866025403784439,
1.,0.866025403784439,1.,0.866025403784439,1.,0.866025403784439,1.,0.866025403784439,
1.,0.866025403784439,1.,0.866025403784439,1.,0.866025403784439,1.,0.866025403784439,
1.,0.866025403784439,1.,0.866025403784439,1.,0.866025403784439,1.,0.866025403784439,
1.,0.866025403784439,1.,0.866025403784439,1.,0.866025403784439,1.,0.866025403784439,
1.,0.866025403784439,1.,0.866025403784439,1.,0.866025403784439,1.,0.866025403784439,
1.,0.866025403784439,1.,0.866025403784439,1.,0.866025403784439,1.,0.866025403784439,
1.,0.866025403784439,1.,0.866025403784439,1.,0.866025403784439,1.,0.866025403784439,
1.,0.866025403784439,1.,0.866025403784439,1.,0.866025403784439,1.,0.866025403784439,
1.,0.866025403784439,1.,0.866025403784439,1.,0.866025403784439,1.,0.866025403784439,
1.,0.866025403784439,1.,0.866025403784439,1.,0.866025403784439,1.,0.866025403784439,
1.,0.866025403784439,1.,0.866025403784439,1.,0.866025403784439,1.,0.866025403784439,
1.,0.866025403784439,1.,0.866025403784439,1.,0.866025403784439,1.,0.866025403784439,
1.,0.866025403784439,1.,0.866025403784439,1.,0.866025403784439,1.,0.866025403784439,
1.,0.866025403784439,1.,0.866025403784439,1.,0.866025403784439,1.,0.866025403784439,
1.,0.866025403784439,1.,0.866025403784439,1.,0.866025403784439,1.,0.866025403784439,
1.,0.866025403784439,1.,0.866025403784439,1.,0.866025403784439,1.,0.866025403784439,
1.,0.866025403784439,1.,0.866025403784439,1.,0.866025403784439,1.,0.866025403784439,
1.,0.866025403784439,1.,0.866025403784439,1.,0.866025403784439,1.,0.866025403784439,
1.,0.866025403784439,1.,0.866025403784439,1.,0.866025403784439,1.,0.866025403784439,
1.,0.866025403784439,1.,0.866025403784439,1.,0.866025403784439,1.,0.866025403784439,
1.,0.866025403784439,1.,0.866025403784439,1.,0.866025403784439,1.,0.866025403784439,
1.,0.866025403784439,1.,0.866025403784439,1.,0.866025403784439,1.,0.866025403784439,
1.,0.866025403784439,1.,0.866025403784439,1.,0.866025403784439,1.,0.866025403784439,
1.,0.866025403784439,1.,0.866025403784439,1.,0.866025403784439,1.,0.866025403784439,
1.,0.866025403784439,1.,0.866025403784439,1.,0.869328783748594,0.993556141390235),
(1.,0.866025403784439,1.,0.866025403784439,1.,0.866025403784439,1.,0.866025403784439,
1.,0.866025403784439,1.,0.866025403784439,1.,0.866025403784439,1.,0.866025403784439,
1.,0.866025403784439,1.,0.866025403784439,1.,0.866025403784439,1.,0.866025403784439,
1.,0.866025403784439,1.,0.866025403784439,1.,0.866025403784439,1.,0.866025403784439,
1.,0.866025403784439,1.,0.866025403784439,1.,0.866025403784439,1.,0.866025403784439,
1.,0.866025403784439,1.,0.866025403784439,1.,0.866025403784439,1.,0.866025403784439,
1.,0.866025403784439,1.,0.866025403784439,1.,0.866025403784439,1.,0.866025403784439,
1.,0.866025403784439,1.,0.866025403784439,1.,0.866025403784439,1.,0.866025403784439,
1.,0.866025403784439,1.,0.866025403784439,1.,0.866025403784439,1.,0.866025403784439,
1.,0.866025403784439,1.,0.866025403784439,1.,0.866025403784439,1.,0.866025403784439,
1.,0.866025403784439,1.,0.866025403784439,1.,0.866025403784439,1.,0.866025403784439,
1.,0.866025403784439,1.,0.866025403784439,1.,0.866025403784439,1.,0.866025403784439,
1.,0.866025403784439,1.,0.866025403784439,1.,0.866025403784439,1.,0.866025403784439,
1.,0.866025403784439,1.,0.866025403784439,1.,0.866025403784439,1.,0.866025403784439,
1.,0.866025403784439,1.,0.866025403784439,1.,0.866025403784439,1.,0.866025403784439,
1.,0.866025403784439,1.,0.866025403784439,1.,0.866025403784439,1.,0.866025403784439,
1.,0.866025403784439,1.,0.866025403784439,1.,0.866025403784439,1.,0.866025403784439,
1.,0.866025403784439,1.,0.866025403784439,1.,0.866025403784439,1.,0.866025403784439,
1.,0.866025403784439,1.,0.866025403784439,1.,0.866025403784439,1.,0.866025403784439,
1.,0.866025403784439,1.,0.866025403784439,1.,0.866025403784439,1.,0.866025403784439,
1.,0.866025403784439,1.,0.866025403784439,1.,0.866025403784439,1.,0.866025403784439,
1.,0.866025403784439,1.,0.866025403784439,1.,0.866025403784439,1.,0.866025403784439,
1.,0.866025403784439,1.,0.866025403784439,1.,0.866025403784439,1.,0.866025403784439,
1.,0.866025403784439,1.,0.866025403784439,1.,0.866025403784439,1.,0.866025403784439,
1.,0.866025403784439,1.,0.866025403784439,1.,0.866025403784439,1.,0.866025403784439,
1.,0.866025403784439,1.,0.866025403784439,1.,0.866025403784439,1.,0.866025403784439,
1.,0.866025403784439,1.,0.866025403784439,1.,0.866025403784439,1.,0.866025403784439,
1.,0.866025403784439,1.,0.866025403784439,1.,0.866025403784439,1.,0.866025403784439,
1.,0.866025403784439,1.,0.866025403784439,1.,0.866025403784439,1.,0.866025403784439,
1.,0.866025403784439,1.,0.866025403784439,1.,0.866025403784439,1.,0.866025403784439,
1.,0.866025403784439,1.,0.866025403784439,1.,0.866025403784439,1.,0.866025403784439,
1.,0.866025403784439,1.,0.866025403784439,1.,0.866025403784439,1.,0.866025403784439,
1.,0.866025403784439,1.,0.866025403784439,1.,0.866025403784439,1.,0.866025403784439,
1.,0.866025403784439,1.,0.866025403784439,1.,0.866025403784439,1.,0.866025403784439,
1.,0.866025403784439,1.,0.866025403784439,1.,0.866025403784439,1.,0.866025403784439,
1.,0.866025403784439,1.,0.866025403784439,1.,0.866025403784439,1.,0.866025403784439,
1.,0.866025403784439,1.,0.866025403784439,1.,0.866025403784439,1.,0.866025403784439,
1.,0.866025403784439,1.,0.866025403784439,1.,0.866025403784439,1.,0.866025403784439,
1.,0.866025403784439,1.,0.866025403784439,1.,0.866025403784439,1.,0.866025403784439,
1.,0.866025403784439,1.,0.866025403784439,1.,0.866025403784439,1.,0.866025403784439,
1.,0.866025403784439,1.,0.866025403784439,1.,0.866025403784439,1.,0.866025403784439,
1.,0.866025403784439,1.,0.866025403784439,1.,0.866025403784439,1.,0.866025403784439,
1.,0.866025403784439,1.,0.866025403784439,1.,0.866025403784439,1.,0.866025403784439,
1.,0.866025403784439,1.,0.866025403784439,1.,0.866025403784439,1.,0.866025403784439,
1.,0.866025403784439,1.,0.866025403784439,1.,0.866025403784439,1.,0.866025403784439,
1.,0.866025403784439,1.,0.866025403784439,1.,0.866025403784439,1.,0.866025403784439,
1.,0.866025403784439,1.,0.866025403784439,1.,0.866025403784439,1.,0.866025403784439,
1.,0.869328783748594,0.993556141390235)))
REPRESENTATION_ITEM('')
SURFACE()
);
#126=(
BOUNDED_SURFACE()
B_SPLINE_SURFACE(3,2,((#31255,#31256,#31257),(#31258,#31259,#31260),(#31261,
#31262,#31263),(#31264,#31265,#31266),(#31267,#31268,#31269),(#31270,#31271,
#31272),(#31273,#31274,#31275),(#31276,#31277,#31278),(#31279,#31280,#31281),
(#31282,#31283,#31284),(#31285,#31286,#31287),(#31288,#31289,#31290),(#31291,
#31292,#31293),(#31294,#31295,#31296),(#31297,#31298,#31299),(#31300,#31301,
#31302),(#31303,#31304,#31305),(#31306,#31307,#31308),(#31309,#31310,#31311),
(#31312,#31313,#31314),(#31315,#31316,#31317),(#31318,#31319,#31320),(#31321,
#31322,#31323),(#31324,#31325,#31326)),.UNSPECIFIED.,.F.,.F.,.F.)
B_SPLINE_SURFACE_WITH_KNOTS((4,2,2,2,2,2,2,2,2,2,2,4),(3,3),(-4.33680868994202E-19,
0.00199566610229966,0.00299349915344949,0.00399133220459933,0.00598699830689899,
0.00698483135804882,0.00748374788362374,0.00773320614641119,0.00785793527780492,
0.00792029984350179,0.00795148212635022,0.00798266440919865),(-8.88988013967173,
1.),.UNSPECIFIED.)
GEOMETRIC_REPRESENTATION_ITEM()
RATIONAL_B_SPLINE_SURFACE(((1.03673130903543,0.997934094247711,1.),(1.03429323702968,
0.998071220506301,1.),(1.03166096458261,0.99821926932168,1.),(1.02743039620336,
0.998457212258636,1.),(1.0259730109093,0.99853918104062,1.),(1.02296180766651,
0.998708542336582,1.),(1.02140250811888,0.998796243156116,1.),(1.01667872310722,
0.999061926435161,1.),(1.0134397522586,0.999244098230379,1.),(1.00845036900139,
0.999524719744889,1.),(1.00676184803489,0.99961968845875,1.),(1.00420736775411,
0.999763361952692,1.),(1.00335516609469,0.999811292950975,1.),(1.00207805691192,
0.999883122332401,1.),(1.00165222462761,0.999907072727549,1.),(1.00101619611475,
0.999942845342188,1.),(1.000804914933,0.999954728583493,1.),(1.00049166224454,
0.99997234708248,1.),(1.00038777606523,0.999978190028486,1.),(1.00023475952815,
0.999986796248967,1.),(1.00018401486096,0.999989650318224,1.),(1.00008917562832,
0.999994984430222,1.),(1.00003836348216,0.999997842294746,1.),(1.00003093298314,
0.999998260213712,1.)))
REPRESENTATION_ITEM('')
SURFACE()
);
#127=(
BOUNDED_SURFACE()
B_SPLINE_SURFACE(3,2,((#31328,#31329,#31330),(#31331,#31332,#31333),(#31334,
#31335,#31336),(#31337,#31338,#31339),(#31340,#31341,#31342),(#31343,#31344,
#31345),(#31346,#31347,#31348),(#31349,#31350,#31351),(#31352,#31353,#31354),
(#31355,#31356,#31357),(#31358,#31359,#31360),(#31361,#31362,#31363),(#31364,
#31365,#31366),(#31367,#31368,#31369),(#31370,#31371,#31372),(#31373,#31374,
#31375)),.UNSPECIFIED.,.F.,.F.,.F.)
B_SPLINE_SURFACE_WITH_KNOTS((4,2,2,2,2,2,2,4),(3,3),(-1.37073647788269E-16,
3.79857431933033E-5,7.59714863867437E-5,0.000151942972773624,0.000303885945547386,
0.000607771891094909,0.00121554378218996,0.00243108756438005),(-0.000101005518536674,
1.),.UNSPECIFIED.)
GEOMETRIC_REPRESENTATION_ITEM()
RATIONAL_B_SPLINE_SURFACE(((1.00000004220253,0.999791088022201,1.),(1.00000004430103,
0.999780699959677,1.),(1.00000006201562,0.999693008760642,1.),(1.00000010657676,
0.999472421084997,1.),(1.00000013303073,0.999341468019306,1.),(1.00000021861,
0.998917831394663,1.),(1.00000028470715,0.998590635693005,1.),(1.00000049900653,
0.997529805625635,1.),(1.00000066545063,0.996705869955465,1.),(1.00000123037801,
0.993909352546599,1.),(1.00000169504325,0.99160915523887,1.),(1.00000335151631,
0.983409241593269,1.),(1.00000480674396,0.976205537946754,1.),(1.00001025390194,
0.949240882635747,1.),(1.00001533088998,0.924108651696566,1.),(1.00002191434951,
0.891519048541741,1.)))
REPRESENTATION_ITEM('')
SURFACE()
);
#128=(
BOUNDED_SURFACE()
B_SPLINE_SURFACE(3,2,((#31377,#31378,#31379),(#31380,#31381,#31382),(#31383,
#31384,#31385),(#31386,#31387,#31388)),.UNSPECIFIED.,.F.,.F.,.F.)
B_SPLINE_SURFACE_WITH_KNOTS((4,4),(3,3),(-1.3918214625889E-5,0.00121512868205196),
(0.,1.00001391821463),.UNSPECIFIED.)
GEOMETRIC_REPRESENTATION_ITEM()
RATIONAL_B_SPLINE_SURFACE(((0.999999999999999,0.891779221283223,1.00000301248005),
(1.,0.884413245314419,1.00000321752252),(1.,0.87579683831728,1.00000345737252),
(1.,0.866200683852581,1.0000037244952)))
REPRESENTATION_ITEM('')
SURFACE()
);
#129=(
BOUNDED_SURFACE()
B_SPLINE_SURFACE(3,2,((#31400,#31401,#31402),(#31403,#31404,#31405),(#31406,
#31407,#31408),(#31409,#31410,#31411),(#31412,#31413,#31414),(#31415,#31416,
#31417),(#31418,#31419,#31420),(#31421,#31422,#31423),(#31424,#31425,#31426),
(#31427,#31428,#31429),(#31430,#31431,#31432),(#31433,#31434,#31435),(#31436,
#31437,#31438),(#31439,#31440,#31441)),.UNSPECIFIED.,.F.,.F.,.F.)
B_SPLINE_SURFACE_WITH_KNOTS((4,2,2,2,2,2,4),(3,3),(0.033103384374427,0.0355583288461946,
0.0367823574217915,0.0380063859973883,0.0392304145729851,0.0404544431485819,
0.0429025002997755),(0.,1.00000688732057),.UNSPECIFIED.)
GEOMETRIC_REPRESENTATION_ITEM()
RATIONAL_B_SPLINE_SURFACE(((1.,0.211850238456311,1.00001085648014),(1.,
0.211789774891773,1.000010857313),(1.,0.211720587176297,1.00001085826604),
(1.,0.21160403471626,1.0000108598715),(1.,0.211562868788471,1.00001086043855),
(1.,0.211477187752812,1.00001086161878),(1.,0.211433005503744,1.00001086222737),
(1.,0.211342033825223,1.00001086348047),(1.,0.211295244231205,1.00001086412498),
(1.,0.211199020809361,1.00001086545043),(1.,0.211149240972151,1.00001086613613),
(1.,0.21099910955097,1.00001086820413),(1.,0.210897693883658,1.0000108696011),
(1.,0.21079496787879,1.00001087101611)))
REPRESENTATION_ITEM('')
SURFACE()
);
#130=(
BOUNDED_SURFACE()
B_SPLINE_SURFACE(3,2,((#31518,#31519,#31520),(#31521,#31522,#31523),(#31524,
#31525,#31526),(#31527,#31528,#31529),(#31530,#31531,#31532),(#31533,#31534,
#31535),(#31536,#31537,#31538),(#31539,#31540,#31541),(#31542,#31543,#31544),
(#31545,#31546,#31547),(#31548,#31549,#31550),(#31551,#31552,#31553),(#31554,
#31555,#31556),(#31557,#31558,#31559),(#31560,#31561,#31562),(#31563,#31564,
#31565),(#31566,#31567,#31568),(#31569,#31570,#31571),(#31572,#31573,#31574),
(#31575,#31576,#31577),(#31578,#31579,#31580),(#31581,#31582,#31583),(#31584,
#31585,#31586),(#31587,#31588,#31589),(#31590,#31591,#31592),(#31593,#31594,
#31595),(#31596,#31597,#31598),(#31599,#31600,#31601),(#31602,#31603,#31604),
(#31605,#31606,#31607),(#31608,#31609,#31610),(#31611,#31612,#31613),(#31614,
#31615,#31616),(#31617,#31618,#31619),(#31620,#31621,#31622),(#31623,#31624,
#31625),(#31626,#31627,#31628),(#31629,#31630,#31631),(#31632,#31633,#31634),
(#31635,#31636,#31637),(#31638,#31639,#31640),(#31641,#31642,#31643),(#31644,
#31645,#31646),(#31647,#31648,#31649),(#31650,#31651,#31652),(#31653,#31654,
#31655),(#31656,#31657,#31658),(#31659,#31660,#31661),(#31662,#31663,#31664),
(#31665,#31666,#31667),(#31668,#31669,#31670),(#31671,#31672,#31673),(#31674,
#31675,#31676),(#31677,#31678,#31679),(#31680,#31681,#31682),(#31683,#31684,
#31685),(#31686,#31687,#31688),(#31689,#31690,#31691),(#31692,#31693,#31694),
(#31695,#31696,#31697),(#31698,#31699,#31700),(#31701,#31702,#31703),(#31704,
#31705,#31706),(#31707,#31708,#31709),(#31710,#31711,#31712),(#31713,#31714,
#31715),(#31716,#31717,#31718),(#31719,#31720,#31721),(#31722,#31723,#31724),
(#31725,#31726,#31727),(#31728,#31729,#31730),(#31731,#31732,#31733),(#31734,
#31735,#31736),(#31737,#31738,#31739),(#31740,#31741,#31742),(#31743,#31744,
#31745)),.UNSPECIFIED.,.F.,.F.,.F.)
B_SPLINE_SURFACE_WITH_KNOTS((4,2,2,2,2,2,2,2,2,2,2,2,2,2,2,2,2,2,2,2,2,
2,2,2,2,2,2,2,2,2,2,2,2,2,2,2,2,4),(3,3),(0.0155469420440516,0.0160999385621218,
0.016652935080192,0.0172059315982622,0.0177589281163324,0.0183119246344026,
0.0188649211524727,0.0194179176705429,0.0199709141886131,0.0210769072247535,
0.0221829002608939,0.0232888932970342,0.0243948863331746,0.025500879369315,
0.0266068724054554,0.0288188584777361,0.0299248515138765,0.0310308445500169,
0.0321368375861573,0.0332428306222976,0.034348823658438,0.0354548166945784,
0.0376668027668591,0.0398787888391399,0.0409847818752803,0.0420907749114206,
0.043196767947561,0.0443027609837014,0.0454087540198418,0.0465147470559821,
0.0470677435740523,0.0476207400921225,0.0481737366101927,0.0487267331282629,
0.0492797296463331,0.0498327261644033,0.0503857226824734,0.0509387192005436),
(0.,1.),.UNSPECIFIED.)
GEOMETRIC_REPRESENTATION_ITEM()
RATIONAL_B_SPLINE_SURFACE(((1.,0.229526735048257,1.),(1.,0.224133558219702,
1.),(1.,0.219259724176961,1.),(1.,0.211064181475465,1.),(1.,0.207811801710184,
1.),(1.,0.203341888285831,1.),(1.,0.202127973482812,1.),(1.,0.201960202180378,
1.),(1.,0.203032258888432,1.),(1.,0.207289559269388,1.),(1.,0.210454353335156,
1.),(1.,0.218450587215706,1.),(1.,0.223279069424003,1.),(1.,0.234195834429115,
1.),(1.,0.240233471751073,1.),(1.,0.252998923243242,1.),(1.,0.259742761586636,
1.),(1.,0.28067947683831,1.),(1.,0.295554256169214,1.),(1.,0.326016231928046,
1.),(1.,0.341634062441765,1.),(1.,0.372564100762139,1.),(1.,0.387951242324607,
1.),(1.,0.418305222299702,1.),(1.,0.433275214730199,1.),(1.,0.46261806682354,
1.),(1.,0.476992506609391,1.),(1.,0.504978264480088,1.),(1.,0.518645722843901,
1.),(1.,0.557478084599559,1.),(1.,0.580701256089758,1.),(1.,0.610367709572221,
1.),(1.,0.619422302565764,1.),(1.,0.635083430287347,1.),(1.,0.64175221457835,
1.),(1.,0.65261413861016,1.),(1.,0.656808227795975,1.),(1.,0.662484548907152,
1.),(1.,0.663913234852522,1.),(1.,0.663922009369197,1.),(1.,0.66252245378572,
1.),(1.,0.656942975295251,1.),(1.,0.652711192029527,1.),(1.,0.636300872830255,
1.),(1.,0.620465569188766,1.),(1.,0.580610974593483,1.),(1.,0.557339096866905,
1.),(1.,0.518721884857682,1.),(1.,0.505222106533921,1.),(1.,0.477115614134931,
1.),(1.,0.462576289466857,1.),(1.,0.433080321145928,1.),(1.,0.418066573341961,
1.),(1.,0.387696762864547,1.),(1.,0.372337606905373,1.),(1.,0.341539686788467,
1.),(1.,0.326093173961657,1.),(1.,0.295606321651459,1.),(1.,0.280553638483726,
1.),(1.,0.25953297193159,1.),(1.,0.252774217996814,1.),(1.,0.240006731870622,
1.),(1.,0.233989040402757,1.),(1.,0.223104380065769,1.),(1.,0.218299068913211,
1.),(1.,0.210355245717533,1.),(1.,0.207219723680965,1.),(1.,0.203010941824996,
1.),(1.,0.201948260378419,1.),(1.,0.202143131871967,1.),(1.,0.203375531025685,
1.),(1.,0.207855714464755,1.),(1.,0.211099729925129,1.),(1.,0.219230361697907,
1.),(1.,0.224140752438636,1.),(1.,0.229539201120578,1.)))
REPRESENTATION_ITEM('')
SURFACE()
);
#131=(
BOUNDED_SURFACE()
B_SPLINE_SURFACE(3,2,((#31822,#31823,#31824),(#31825,#31826,#31827),(#31828,
#31829,#31830),(#31831,#31832,#31833),(#31834,#31835,#31836),(#31837,#31838,
#31839),(#31840,#31841,#31842),(#31843,#31844,#31845),(#31846,#31847,#31848),
(#31849,#31850,#31851),(#31852,#31853,#31854),(#31855,#31856,#31857),(#31858,
#31859,#31860),(#31861,#31862,#31863)),.UNSPECIFIED.,.F.,.F.,.F.)
B_SPLINE_SURFACE_WITH_KNOTS((4,2,2,2,2,2,4),(3,3),(0.0331033843745195,0.0355583288461946,
0.0367823574217914,0.0380063859973882,0.039230414572985,0.0404544431485818,
0.0429025002997754),(-6.88732048148063E-6,1.),.UNSPECIFIED.)
GEOMETRIC_REPRESENTATION_ITEM()
RATIONAL_B_SPLINE_SURFACE(((1.00001085647999,0.211850238456374,0.999999999999999),
(1.00001085731285,0.211789774892188,1.),(1.00001085826589,0.211720587175911,
1.),(1.00001085987136,0.211604034716559,1.),(1.0000108604384,0.211562868788407,
1.),(1.00001086161863,0.211477187753023,1.),(1.00001086222722,0.211433005503953,
1.),(1.00001086348033,0.21134203382516,1.),(1.00001086412484,0.211295244231278,
1.),(1.00001086545028,0.211199020809434,1.),(1.00001086613598,0.211149240972224,
1.),(1.00001086820399,0.210999109551043,1.),(1.00001086960095,0.21089769388373,
1.),(1.00001087101596,0.210794967878863,1.)))
REPRESENTATION_ITEM('')
SURFACE()
);
#132=(
BOUNDED_SURFACE()
B_SPLINE_SURFACE(3,2,((#31872,#31873,#31874),(#31875,#31876,#31877),(#31878,
#31879,#31880),(#31881,#31882,#31883)),.UNSPECIFIED.,.F.,.F.,.F.)
B_SPLINE_SURFACE_WITH_KNOTS((4,4),(3,3),(-1.39182146545714E-5,0.00121512868208074),
(0.,1.00001391821465),.UNSPECIFIED.)
GEOMETRIC_REPRESENTATION_ITEM()
RATIONAL_B_SPLINE_SURFACE(((1.,0.866200683851906,1.00000372449521),(1.,
0.875796838317096,1.00000345737253),(1.,0.884413245314652,1.00000321752253),
(1.,0.891779221283738,1.00000301248006)))
REPRESENTATION_ITEM('')
SURFACE()
);
#133=(
BOUNDED_SURFACE()
B_SPLINE_SURFACE(3,2,((#31885,#31886,#31887),(#31888,#31889,#31890),(#31891,
#31892,#31893),(#31894,#31895,#31896),(#31897,#31898,#31899),(#31900,#31901,
#31902),(#31903,#31904,#31905),(#31906,#31907,#31908),(#31909,#31910,#31911),
(#31912,#31913,#31914),(#31915,#31916,#31917),(#31918,#31919,#31920),(#31921,
#31922,#31923),(#31924,#31925,#31926)),.UNSPECIFIED.,.F.,.F.,.F.)
B_SPLINE_SURFACE_WITH_KNOTS((4,2,2,2,2,2,4),(3,3),(-0.000142750203022182,
0.00120936219001056,0.00181404328501584,0.00211638383251848,0.0022675541062698,
0.00234313924314546,0.0025614745830495),(-0.00757884796103774,1.),
 .UNSPECIFIED.)
GEOMETRIC_REPRESENTATION_ITEM()
RATIONAL_B_SPLINE_SURFACE(((1.00183804612443,0.878738422126962,1.),(1.00124990939078,
0.917539618342774,1.),(1.00080710421406,0.946752843030485,1.),(1.00036309214798,
0.976045689935564,1.),(1.00025309503348,0.983302539200046,1.),(1.00012791013031,
0.991561373775666,1.),(1.00009280627034,0.993877283802622,1.),(1.00005012171262,
0.996693315865673,1.),(1.00003753469437,0.997523720322227,1.),(1.00002137280872,
0.998589969819041,1.),(1.00001641874054,0.998916804993093,1.),(0.999999713951067,
1.00001887153131,1.),(0.999989596975289,1.00068631965997,1.),(1.00005723328726,
0.996224143329086,0.999999999999999)))
REPRESENTATION_ITEM('')
SURFACE()
);
#134=(
BOUNDED_SURFACE()
B_SPLINE_SURFACE(3,2,((#31928,#31929,#31930),(#31931,#31932,#31933),(#31934,
#31935,#31936),(#31937,#31938,#31939),(#31940,#31941,#31942),(#31943,#31944,
#31945),(#31946,#31947,#31948),(#31949,#31950,#31951),(#31952,#31953,#31954),
(#31955,#31956,#31957),(#31958,#31959,#31960),(#31961,#31962,#31963),(#31964,
#31965,#31966),(#31967,#31968,#31969),(#31970,#31971,#31972),(#31973,#31974,
#31975),(#31976,#31977,#31978),(#31979,#31980,#31981),(#31982,#31983,#31984),
(#31985,#31986,#31987),(#31988,#31989,#31990),(#31991,#31992,#31993),(#31994,
#31995,#31996),(#31997,#31998,#31999)),.UNSPECIFIED.,.F.,.F.,.F.)
B_SPLINE_SURFACE_WITH_KNOTS((4,2,2,2,2,2,2,2,2,2,2,4),(3,3),(0.,0.00199566610230272,
0.00299349915345408,0.00399133220460544,0.00598699830690816,0.00698483135805952,
0.0074837478836352,0.00773320614642304,0.00785793527781696,0.00792029984351392,
0.0079514821263624,0.00798266440921088),(0.,9.4347309660509),
 .UNSPECIFIED.)
GEOMETRIC_REPRESENTATION_ITEM()
RATIONAL_B_SPLINE_SURFACE(((1.,0.998029170758512,1.03324682886395),(1.,
0.99815998623251,1.03104004220522),(1.,0.998301221588568,1.02865747774274),
(1.,0.998528213985216,1.02482823814861),(1.,0.99860641042422,1.0235091062976),
(1.,0.998767977423409,1.0207835579553),(1.,0.998851642101808,1.01937217984798),
(1.,0.999105098182627,1.01509651214116),(1.,0.999278886120722,1.01216480313518),
(1.,0.999546592953898,1.00764873290395),(1.,0.999637191045363,1.00612039184888),
(1.,0.999774252439753,1.00380823987384),(1.,0.999819977571642,1.00303688150212),
(1.,0.999888501242266,1.00188092404907),(1.,0.999911349399373,1.00149548793254),
(1.,0.99994547569713,1.00091979565164),(1.,0.999956812051398,1.00072855745488),
(1.,0.999973619716972,1.0004450211803),(1.,0.999979193760625,1.00035099006309),
(1.,0.999987403908142,1.0002124892921),(1.,0.999990126628257,1.00016655846877),
(1.,0.999995215255311,1.00008071606839),(1.,0.999997941596032,1.00003472416737),
(1.,0.999998340281648,1.00002799855556)))
REPRESENTATION_ITEM('')
SURFACE()
);
#135=(
BOUNDED_SURFACE()
B_SPLINE_SURFACE(3,2,((#32683,#32684,#32685),(#32686,#32687,#32688),(#32689,
#32690,#32691),(#32692,#32693,#32694),(#32695,#32696,#32697),(#32698,#32699,
#32700),(#32701,#32702,#32703),(#32704,#32705,#32706),(#32707,#32708,#32709),
(#32710,#32711,#32712),(#32713,#32714,#32715),(#32716,#32717,#32718),(#32719,
#32720,#32721),(#32722,#32723,#32724),(#32725,#32726,#32727),(#32728,#32729,
#32730),(#32731,#32732,#32733),(#32734,#32735,#32736),(#32737,#32738,#32739),
(#32740,#32741,#32742),(#32743,#32744,#32745),(#32746,#32747,#32748)),
 .UNSPECIFIED.,.F.,.F.,.F.)
B_SPLINE_SURFACE_WITH_KNOTS((4,2,2,2,2,2,2,2,2,2,4),(3,3),(0.00881272913566369,
0.00928844068390005,0.00953838644963798,0.00978833221537591,0.0100382779811138,
0.0105381695125897,0.0110380610440656,0.0120378441070173,0.0125377356384932,
0.0127876814042311,0.01326339295247),(-0.00102566064560791,1.),
 .UNSPECIFIED.)
GEOMETRIC_REPRESENTATION_ITEM()
RATIONAL_B_SPLINE_SURFACE(((1.00132329066919,0.354908139032077,1.),(1.00124812393843,
0.391551219315617,1.),(1.00115915858371,0.434921000104149,1.),(1.00102358876472,
0.501010022609669,1.),(1.00097653790903,0.523946875988812,1.),(1.00088693501083,
0.567627453274935,1.),(1.00084389129738,0.588610862181495,1.),(1.00076096626522,
0.629036042047148,1.),(1.00072089412048,0.648570838919578,1.),(1.00060683104295,
0.704175525527758,1.),(1.00053863758583,0.737419199938388,1.),(1.00041471240488,
0.797831569997033,1.),(1.00035895931741,0.825010680216488,1.),(1.00021007792585,
0.897588970214807,1.),(1.00013587466058,0.933762370057051,1.),(1.00006032673641,
0.970591278572527,1.),(1.00004117816685,0.979926027666627,1.),(1.00002165568508,
0.989443055473061,1.),(1.00001667885161,0.991869215376876,1.),(1.00000682799133,
0.99667141789903,1.),(1.00000607453102,0.997038722775045,1.),(1.00001271218793,
0.993802926931325,1.)))
REPRESENTATION_ITEM('')
SURFACE()
);
#136=(
BOUNDED_SURFACE()
B_SPLINE_SURFACE(3,2,((#32822,#32823,#32824),(#32825,#32826,#32827),(#32828,
#32829,#32830),(#32831,#32832,#32833),(#32834,#32835,#32836),(#32837,#32838,
#32839),(#32840,#32841,#32842),(#32843,#32844,#32845),(#32846,#32847,#32848),
(#32849,#32850,#32851),(#32852,#32853,#32854),(#32855,#32856,#32857),(#32858,
#32859,#32860),(#32861,#32862,#32863),(#32864,#32865,#32866),(#32867,#32868,
#32869),(#32870,#32871,#32872),(#32873,#32874,#32875),(#32876,#32877,#32878),
(#32879,#32880,#32881),(#32882,#32883,#32884),(#32885,#32886,#32887),(#32888,
#32889,#32890),(#32891,#32892,#32893),(#32894,#32895,#32896),(#32897,#32898,
#32899),(#32900,#32901,#32902),(#32903,#32904,#32905)),.UNSPECIFIED.,.F.,
 .F.,.F.)
B_SPLINE_SURFACE_WITH_KNOTS((4,2,2,2,2,2,2,2,2,2,2,2,2,4),(3,3),(0.0120978781599544,
0.013608206651586,0.0151185351432177,0.0158736993890335,0.0166288636348494,
0.0173840278806652,0.018139192126481,0.0188943563722969,0.0196495206181127,
0.0204046848639285,0.0211598491097444,0.0219150133555602,0.022670177601376,
0.0241805060930077),(0.,1.00005676629322),.UNSPECIFIED.)
GEOMETRIC_REPRESENTATION_ITEM()
RATIONAL_B_SPLINE_SURFACE(((1.,0.419714375858336,1.00006588132778),(1.,
0.455258548961405,1.00006184590587),(1.,0.490259453324333,1.00005787216267),
(1.,0.554227398223351,1.00005060971644),(1.,0.583234396585999,1.00004731647689),
(1.,0.620852932125695,1.00004304554726),(1.,0.632335513594305,1.00004174190008),
(1.,0.652343207191375,1.00003947037488),(1.,0.660962788243787,1.00003849177155),
(1.,0.67512712292899,1.000036883658),(1.,0.680682058163542,1.00003625299183),
(1.,0.688032273240624,1.0000354185029),(1.,0.689900381447712,1.00003520641175),
(1.,0.689947597716664,1.00003520105116),(1.,0.688072411855674,1.00003541394586),
(1.,0.680752669873931,1.0000362449751),(1.,0.675339625853613,1.00003685953199),
(1.,0.661242565913974,1.00003846000767),(1.,0.652474855221301,1.00003945542854),
(1.,0.632370855573539,1.00004173788762),(1.,0.621020695612542,1.00004302650063),
(1.,0.596023875522447,1.00004586445427),(1.,0.582284387510476,1.00004742433388),
(1.,0.553320360279571,1.00005071269481),(1.,0.538073094759082,1.0000524437563),
(1.,0.490378194191559,1.00005785868172),(1.,0.455940368475232,1.00006176849714),
(1.,0.419656970284633,1.00006588784518)))
REPRESENTATION_ITEM('')
SURFACE()
);
#137=(
BOUNDED_SURFACE()
B_SPLINE_SURFACE(3,2,((#32908,#32909,#32910),(#32911,#32912,#32913),(#32914,
#32915,#32916),(#32917,#32918,#32919),(#32920,#32921,#32922),(#32923,#32924,
#32925),(#32926,#32927,#32928),(#32929,#32930,#32931),(#32932,#32933,#32934),
(#32935,#32936,#32937),(#32938,#32939,#32940),(#32941,#32942,#32943),(#32944,
#32945,#32946),(#32947,#32948,#32949),(#32950,#32951,#32952),(#32953,#32954,
#32955),(#32956,#32957,#32958),(#32959,#32960,#32961),(#32962,#32963,#32964),
(#32965,#32966,#32967),(#32968,#32969,#32970),(#32971,#32972,#32973)),
 .UNSPECIFIED.,.F.,.F.,.F.)
B_SPLINE_SURFACE_WITH_KNOTS((4,2,2,2,2,2,2,2,2,2,4),(3,3),(0.0086385816929815,
0.00928844068390017,0.00953838644963812,0.00978833221537607,0.010038277981114,
0.0105381695125899,0.0110380610440658,0.0120378441070176,0.0125377356384935,
0.0127876814042315,0.0134375403951501),(0.,1.00153795011474),
 .UNSPECIFIED.)
GEOMETRIC_REPRESENTATION_ITEM()
RATIONAL_B_SPLINE_SURFACE(((1.,0.317352891590616,1.0020997543974),(1.,0.359464191769642,
1.00197022423952),(1.,0.418763269709159,1.00178782619208),(1.,0.50075465721736,
1.00153562886443),(1.,0.523703248865329,1.00146504128611),(1.,0.567406180323521,
1.00133061542921),(1.,0.588400327795338,1.00126603952618),(1.,0.628846195835825,
1.0011416320714),(1.,0.648390989925248,1.00108151423477),(1.,0.704024133042094,
1.00091039223709),(1.,0.737284820387534,1.00080808568126),(1.,0.797728107356911,
1.000622168161),(1.,0.82492112688211,1.000538525146),(1.,0.897536559877894,
1.00031516731898),(1.,0.933728471984707,1.00020384460823),(1.,0.970576228230773,
1.00009050458634),(1.,0.97991575451876,1.00006177713528),(1.,0.98943765280286,
1.00003248872617),(1.,0.991865054329365,1.00002502228126),(1.,0.997822764595849,
1.00000669695888),(1.,0.996933411986155,1.00000943251877),(1.,0.988754588874827,
1.00003458976266)))
REPRESENTATION_ITEM('')
SURFACE()
);
#138=B_SPLINE_SURFACE_WITH_KNOTS('',1,3,((#28118,#28119,#28120,#28121,#28122,
#28123,#28124,#28125,#28126,#28127,#28128,#28129,#28130,#28131,#28132,#28133,
#28134,#28135,#28136,#28137,#28138,#28139,#28140,#28141,#28142,#28143,#28144,
#28145,#28146,#28147,#28148,#28149,#28150,#28151,#28152,#28153,#28154,#28155,
#28156,#28157,#28158,#28159,#28160,#28161,#28162,#28163,#28164,#28165,#28166,
#28167,#28168,#28169,#28170,#28171),(#28172,#28173,#28174,#28175,#28176,
#28177,#28178,#28179,#28180,#28181,#28182,#28183,#28184,#28185,#28186,#28187,
#28188,#28189,#28190,#28191,#28192,#28193,#28194,#28195,#28196,#28197,#28198,
#28199,#28200,#28201,#28202,#28203,#28204,#28205,#28206,#28207,#28208,#28209,
#28210,#28211,#28212,#28213,#28214,#28215,#28216,#28217,#28218,#28219,#28220,
#28221,#28222,#28223,#28224,#28225)),.UNSPECIFIED.,.F.,.F.,.F.,(2,2),(4,
2,2,2,2,2,2,2,2,2,2,2,2,2,2,2,2,2,2,2,2,2,2,2,2,2,4),(-0.00171316499800555,
1.),(-0.00171316499800555,0.015625,0.0234375,0.02734375,0.03125,0.046875,
0.0546875,0.0625,0.09375,0.125,0.1875,0.25,0.5,0.625,0.75,0.8125,0.84375,
0.875,0.90625,0.921875,0.9296875,0.9375,0.953125,0.9609375,0.96484375,0.96875,
1.00171316499801),.UNSPECIFIED.);
#139=B_SPLINE_SURFACE_WITH_KNOTS('',1,3,((#28230,#28231,#28232,#28233,#28234,
#28235,#28236,#28237,#28238,#28239,#28240,#28241,#28242,#28243,#28244,#28245,
#28246,#28247,#28248,#28249,#28250,#28251,#28252,#28253,#28254,#28255,#28256,
#28257,#28258,#28259,#28260,#28261,#28262,#28263,#28264,#28265,#28266,#28267,
#28268,#28269,#28270,#28271,#28272,#28273,#28274,#28275,#28276,#28277,#28278,
#28279,#28280,#28281,#28282,#28283),(#28284,#28285,#28286,#28287,#28288,
#28289,#28290,#28291,#28292,#28293,#28294,#28295,#28296,#28297,#28298,#28299,
#28300,#28301,#28302,#28303,#28304,#28305,#28306,#28307,#28308,#28309,#28310,
#28311,#28312,#28313,#28314,#28315,#28316,#28317,#28318,#28319,#28320,#28321,
#28322,#28323,#28324,#28325,#28326,#28327,#28328,#28329,#28330,#28331,#28332,
#28333,#28334,#28335,#28336,#28337)),.UNSPECIFIED.,.F.,.F.,.F.,(2,2),(4,
2,2,2,2,2,2,2,2,2,2,2,2,2,2,2,2,2,2,2,2,2,2,2,2,2,4),(-0.0017131650178696,
1.),(-0.00171316501786942,0.015625,0.0234375,0.02734375,0.03125,0.046875,
0.0546875,0.0625,0.09375,0.125,0.1875,0.25,0.5,0.625,0.75,0.8125,0.84375,
0.875,0.90625,0.921875,0.9296875,0.9375,0.953125,0.9609375,0.96484375,0.96875,
1.00171316501787),.UNSPECIFIED.);
#140=TOROIDAL_SURFACE('',#17973,11.5,1.00000000000001);
#141=TOROIDAL_SURFACE('',#17983,22.75,2.25);
#142=TOROIDAL_SURFACE('',#18022,2.5,0.5);
#143=TOROIDAL_SURFACE('',#18027,2.5,0.5);
#144=TOROIDAL_SURFACE('',#18037,8.,2.);
#145=TOROIDAL_SURFACE('',#18066,7.,0.999999999999999);
#146=TOROIDAL_SURFACE('',#18072,8.,2.);
#147=TOROIDAL_SURFACE('',#18113,9.51643315533714,1.);
#148=TOROIDAL_SURFACE('',#18120,9.51643315533713,1.);
#149=TOROIDAL_SURFACE('',#18150,6.,0.5);
#150=TOROIDAL_SURFACE('',#18161,5.48772230081581,1.23243402184158);
#151=TOROIDAL_SURFACE('',#18192,5.40661052483917,0.5);
#152=TOROIDAL_SURFACE('',#18193,6.,0.5);
#153=TOROIDAL_SURFACE('',#18194,5.40661052483917,0.5);
#154=TOROIDAL_SURFACE('',#18219,10.5,2.);
#155=TOROIDAL_SURFACE('',#18245,8.00000000000022,2.);
#156=TOROIDAL_SURFACE('',#18253,8.,2.);
#157=TOROIDAL_SURFACE('',#18258,8.00000000000095,2.);
#158=TOROIDAL_SURFACE('',#18266,8.00000000000152,2.);
#159=TOROIDAL_SURFACE('',#18274,8.00000000000143,2.);
#160=TOROIDAL_SURFACE('',#18279,8.00000000000082,2.);
#161=TOROIDAL_SURFACE('',#18314,23.,2.);
#162=TOROIDAL_SURFACE('',#18318,23.,2.);
#163=TOROIDAL_SURFACE('',#18322,23.,2.);
#164=TOROIDAL_SURFACE('',#18326,23.,2.);
#165=TOROIDAL_SURFACE('',#18330,23.,2.);
#166=TOROIDAL_SURFACE('',#18335,23.,2.);
#167=TOROIDAL_SURFACE('',#18339,23.,2.);
#168=TOROIDAL_SURFACE('',#18343,23.,2.);
#169=TOROIDAL_SURFACE('',#18347,23.,2.);
#170=TOROIDAL_SURFACE('',#18351,23.,2.);
#171=TOROIDAL_SURFACE('',#18369,23.,2.);
#172=TOROIDAL_SURFACE('',#18372,23.,2.);
#173=TOROIDAL_SURFACE('',#18384,8.00000000000082,2.);
#174=TOROIDAL_SURFACE('',#18397,8.00000000000143,2.);
#175=TOROIDAL_SURFACE('',#18407,8.00000000000152,2.);
#176=TOROIDAL_SURFACE('',#18411,8.00000000000095,2.);
#177=TOROIDAL_SURFACE('',#18433,8.,2.);
#178=TOROIDAL_SURFACE('',#18446,8.00000000000022,2.);
#179=TOROIDAL_SURFACE('',#18545,3.3,0.3);
#180=TOROIDAL_SURFACE('',#18563,3.3,0.3);
#181=TOROIDAL_SURFACE('',#18597,1.1,0.1);
#182=TOROIDAL_SURFACE('',#18602,1.1,0.1);
#183=TOROIDAL_SURFACE('',#18656,2.5,0.5);
#184=TOROIDAL_SURFACE('',#19189,1.81782234903766,0.9);
#185=TOROIDAL_SURFACE('',#19210,4.5,0.5);
#186=(
BOUNDED_CURVE()
B_SPLINE_CURVE(2,(#24977,#24978,#24979,#24980,#24981,#24982,#24983),
 .UNSPECIFIED.,.F.,.F.)
B_SPLINE_CURVE_WITH_KNOTS((3,2,2,3),(0.,0.00520833333333333,0.0104166666666667,
0.015625),.UNSPECIFIED.)
CURVE()
GEOMETRIC_REPRESENTATION_ITEM()
RATIONAL_B_SPLINE_CURVE((1.,0.866025403784439,1.,0.866025403784439,1.,0.866025403784439,
1.))
REPRESENTATION_ITEM('')
);
#187=(
BOUNDED_CURVE()
B_SPLINE_CURVE(2,(#24986,#24987,#24988,#24989,#24990,#24991,#24992),
 .UNSPECIFIED.,.F.,.F.)
B_SPLINE_CURVE_WITH_KNOTS((3,2,2,3),(0.,0.00520833333333333,0.0104166666666667,
0.015625),.UNSPECIFIED.)
CURVE()
GEOMETRIC_REPRESENTATION_ITEM()
RATIONAL_B_SPLINE_CURVE((1.,0.866025403784439,1.,0.866025403784439,1.,0.866025403784439,
1.))
REPRESENTATION_ITEM('')
);
#188=(
BOUNDED_CURVE()
B_SPLINE_CURVE(2,(#24997,#24998,#24999,#25000,#25001,#25002,#25003,#25004,
#25005,#25006,#25007,#25008,#25009),.UNSPECIFIED.,.F.,.F.)
B_SPLINE_CURVE_WITH_KNOTS((3,2,2,2,2,2,3),(0.015625,0.0208333333333333,
0.0260416666666667,0.03125,0.0364583333333333,0.0416666666666667,0.046875),
 .UNSPECIFIED.)
CURVE()
GEOMETRIC_REPRESENTATION_ITEM()
RATIONAL_B_SPLINE_CURVE((1.,0.866025403784439,1.,0.866025403784439,1.,0.866025403784439,
1.,0.866025403784439,1.,0.866025403784439,1.,0.866025403784439,1.))
REPRESENTATION_ITEM('')
);
#189=(
BOUNDED_CURVE()
B_SPLINE_CURVE(2,(#25010,#25011,#25012,#25013,#25014,#25015,#25016,#25017,
#25018,#25019,#25020,#25021,#25022),.UNSPECIFIED.,.F.,.F.)
B_SPLINE_CURVE_WITH_KNOTS((3,2,2,2,2,2,3),(0.015625,0.0208333333333333,
0.0260416666666667,0.03125,0.0364583333333333,0.0416666666666667,0.046875),
 .UNSPECIFIED.)
CURVE()
GEOMETRIC_REPRESENTATION_ITEM()
RATIONAL_B_SPLINE_CURVE((1.,0.866025403784439,1.,0.866025403784439,1.,0.866025403784439,
1.,0.866025403784439,1.,0.866025403784439,1.,0.866025403784439,1.))
REPRESENTATION_ITEM('')
);
#190=(
BOUNDED_CURVE()
B_SPLINE_CURVE(2,(#25027,#25028,#25029,#25030,#25031,#25032,#25033,#25034,
#25035,#25036,#25037,#25038,#25039),.UNSPECIFIED.,.F.,.F.)
B_SPLINE_CURVE_WITH_KNOTS((3,2,2,2,2,2,3),(0.046875,0.0520833333333333,
0.0572916666666667,0.0625,0.0677083333333333,0.0729166666666667,0.078125),
 .UNSPECIFIED.)
CURVE()
GEOMETRIC_REPRESENTATION_ITEM()
RATIONAL_B_SPLINE_CURVE((1.,0.866025403784439,1.,0.866025403784439,1.,0.866025403784439,
1.,0.866025403784439,1.,0.866025403784439,1.,0.866025403784439,1.))
REPRESENTATION_ITEM('')
);
#191=(
BOUNDED_CURVE()
B_SPLINE_CURVE(2,(#25040,#25041,#25042,#25043,#25044,#25045,#25046,#25047,
#25048,#25049,#25050,#25051,#25052),.UNSPECIFIED.,.F.,.F.)
B_SPLINE_CURVE_WITH_KNOTS((3,2,2,2,2,2,3),(0.046875,0.0520833333333333,
0.0572916666666667,0.0625,0.0677083333333333,0.0729166666666667,0.078125),
 .UNSPECIFIED.)
CURVE()
GEOMETRIC_REPRESENTATION_ITEM()
RATIONAL_B_SPLINE_CURVE((1.,0.866025403784439,1.,0.866025403784439,1.,0.866025403784439,
1.,0.866025403784439,1.,0.866025403784439,1.,0.866025403784439,1.))
REPRESENTATION_ITEM('')
);
#192=(
BOUNDED_CURVE()
B_SPLINE_CURVE(2,(#25057,#25058,#25059,#25060,#25061,#25062,#25063,#25064,
#25065,#25066,#25067,#25068,#25069),.UNSPECIFIED.,.F.,.F.)
B_SPLINE_CURVE_WITH_KNOTS((3,2,2,2,2,2,3),(0.078125,0.0833333333333333,
0.0885416666666667,0.09375,0.0989583333333333,0.104166666666667,0.109375),
 .UNSPECIFIED.)
CURVE()
GEOMETRIC_REPRESENTATION_ITEM()
RATIONAL_B_SPLINE_CURVE((1.,0.866025403784439,1.,0.866025403784439,1.,0.866025403784439,
1.,0.866025403784439,1.,0.866025403784439,1.,0.866025403784439,1.))
REPRESENTATION_ITEM('')
);
#193=(
BOUNDED_CURVE()
B_SPLINE_CURVE(2,(#25070,#25071,#25072,#25073,#25074,#25075,#25076,#25077,
#25078,#25079,#25080,#25081,#25082),.UNSPECIFIED.,.F.,.F.)
B_SPLINE_CURVE_WITH_KNOTS((3,2,2,2,2,2,3),(0.078125,0.0833333333333333,
0.0885416666666667,0.09375,0.0989583333333333,0.104166666666667,0.109375),
 .UNSPECIFIED.)
CURVE()
GEOMETRIC_REPRESENTATION_ITEM()
RATIONAL_B_SPLINE_CURVE((1.,0.866025403784439,1.,0.866025403784439,1.,0.866025403784439,
1.,0.866025403784439,1.,0.866025403784439,1.,0.866025403784439,1.))
REPRESENTATION_ITEM('')
);
#194=(
BOUNDED_CURVE()
B_SPLINE_CURVE(2,(#25087,#25088,#25089,#25090,#25091,#25092,#25093,#25094,
#25095,#25096,#25097,#25098,#25099),.UNSPECIFIED.,.F.,.F.)
B_SPLINE_CURVE_WITH_KNOTS((3,2,2,2,2,2,3),(0.109375,0.114583333333333,0.119791666666667,
0.125,0.130208333333333,0.135416666666667,0.140625),.UNSPECIFIED.)
CURVE()
GEOMETRIC_REPRESENTATION_ITEM()
RATIONAL_B_SPLINE_CURVE((1.,0.866025403784439,1.,0.866025403784439,1.,0.866025403784439,
1.,0.866025403784439,1.,0.866025403784439,1.,0.866025403784439,1.))
REPRESENTATION_ITEM('')
);
#195=(
BOUNDED_CURVE()
B_SPLINE_CURVE(2,(#25100,#25101,#25102,#25103,#25104,#25105,#25106,#25107,
#25108,#25109,#25110,#25111,#25112),.UNSPECIFIED.,.F.,.F.)
B_SPLINE_CURVE_WITH_KNOTS((3,2,2,2,2,2,3),(0.109375,0.114583333333333,0.119791666666667,
0.125,0.130208333333333,0.135416666666667,0.140625),.UNSPECIFIED.)
CURVE()
GEOMETRIC_REPRESENTATION_ITEM()
RATIONAL_B_SPLINE_CURVE((1.,0.866025403784439,1.,0.866025403784439,1.,0.866025403784439,
1.,0.866025403784439,1.,0.866025403784439,1.,0.866025403784439,1.))
REPRESENTATION_ITEM('')
);
#196=(
BOUNDED_CURVE()
B_SPLINE_CURVE(2,(#25117,#25118,#25119,#25120,#25121,#25122,#25123,#25124,
#25125,#25126,#25127,#25128,#25129),.UNSPECIFIED.,.F.,.F.)
B_SPLINE_CURVE_WITH_KNOTS((3,2,2,2,2,2,3),(0.140625,0.145833333333333,0.151041666666667,
0.15625,0.161458333333333,0.166666666666667,0.171875),.UNSPECIFIED.)
CURVE()
GEOMETRIC_REPRESENTATION_ITEM()
RATIONAL_B_SPLINE_CURVE((1.,0.866025403784439,1.,0.866025403784439,1.,0.866025403784439,
1.,0.866025403784439,1.,0.866025403784439,1.,0.866025403784439,1.))
REPRESENTATION_ITEM('')
);
#197=(
BOUNDED_CURVE()
B_SPLINE_CURVE(2,(#25130,#25131,#25132,#25133,#25134,#25135,#25136,#25137,
#25138,#25139,#25140,#25141,#25142),.UNSPECIFIED.,.F.,.F.)
B_SPLINE_CURVE_WITH_KNOTS((3,2,2,2,2,2,3),(0.140625,0.145833333333333,0.151041666666667,
0.15625,0.161458333333333,0.166666666666667,0.171875),.UNSPECIFIED.)
CURVE()
GEOMETRIC_REPRESENTATION_ITEM()
RATIONAL_B_SPLINE_CURVE((1.,0.866025403784439,1.,0.866025403784439,1.,0.866025403784439,
1.,0.866025403784439,1.,0.866025403784439,1.,0.866025403784439,1.))
REPRESENTATION_ITEM('')
);
#198=(
BOUNDED_CURVE()
B_SPLINE_CURVE(2,(#25147,#25148,#25149,#25150,#25151,#25152,#25153,#25154,
#25155,#25156,#25157,#25158,#25159),.UNSPECIFIED.,.F.,.F.)
B_SPLINE_CURVE_WITH_KNOTS((3,2,2,2,2,2,3),(0.171875,0.177083333333333,0.182291666666667,
0.1875,0.192708333333333,0.197916666666667,0.203125),.UNSPECIFIED.)
CURVE()
GEOMETRIC_REPRESENTATION_ITEM()
RATIONAL_B_SPLINE_CURVE((1.,0.866025403784439,1.,0.866025403784439,1.,0.866025403784439,
1.,0.866025403784439,1.,0.866025403784439,1.,0.866025403784439,1.))
REPRESENTATION_ITEM('')
);
#199=(
BOUNDED_CURVE()
B_SPLINE_CURVE(2,(#25160,#25161,#25162,#25163,#25164,#25165,#25166,#25167,
#25168,#25169,#25170,#25171,#25172),.UNSPECIFIED.,.F.,.F.)
B_SPLINE_CURVE_WITH_KNOTS((3,2,2,2,2,2,3),(0.171875,0.177083333333333,0.182291666666667,
0.1875,0.192708333333333,0.197916666666667,0.203125),.UNSPECIFIED.)
CURVE()
GEOMETRIC_REPRESENTATION_ITEM()
RATIONAL_B_SPLINE_CURVE((1.,0.866025403784439,1.,0.866025403784439,1.,0.866025403784439,
1.,0.866025403784439,1.,0.866025403784439,1.,0.866025403784439,1.))
REPRESENTATION_ITEM('')
);
#200=(
BOUNDED_CURVE()
B_SPLINE_CURVE(2,(#25177,#25178,#25179,#25180,#25181,#25182,#25183,#25184,
#25185,#25186,#25187,#25188,#25189),.UNSPECIFIED.,.F.,.F.)
B_SPLINE_CURVE_WITH_KNOTS((3,2,2,2,2,2,3),(0.203125,0.208333333333333,0.213541666666667,
0.21875,0.223958333333333,0.229166666666667,0.234375),.UNSPECIFIED.)
CURVE()
GEOMETRIC_REPRESENTATION_ITEM()
RATIONAL_B_SPLINE_CURVE((1.,0.866025403784439,1.,0.866025403784439,1.,0.866025403784439,
1.,0.866025403784439,1.,0.866025403784439,1.,0.866025403784439,1.))
REPRESENTATION_ITEM('')
);
#201=(
BOUNDED_CURVE()
B_SPLINE_CURVE(2,(#25190,#25191,#25192,#25193,#25194,#25195,#25196,#25197,
#25198,#25199,#25200,#25201,#25202),.UNSPECIFIED.,.F.,.F.)
B_SPLINE_CURVE_WITH_KNOTS((3,2,2,2,2,2,3),(0.203125,0.208333333333333,0.213541666666667,
0.21875,0.223958333333333,0.229166666666667,0.234375),.UNSPECIFIED.)
CURVE()
GEOMETRIC_REPRESENTATION_ITEM()
RATIONAL_B_SPLINE_CURVE((1.,0.866025403784439,1.,0.866025403784439,1.,0.866025403784439,
1.,0.866025403784439,1.,0.866025403784439,1.,0.866025403784439,1.))
REPRESENTATION_ITEM('')
);
#202=(
BOUNDED_CURVE()
B_SPLINE_CURVE(2,(#25207,#25208,#25209,#25210,#25211,#25212,#25213,#25214,
#25215,#25216,#25217,#25218,#25219),.UNSPECIFIED.,.F.,.F.)
B_SPLINE_CURVE_WITH_KNOTS((3,2,2,2,2,2,3),(0.234375,0.239583333333333,0.244791666666667,
0.25,0.255208333333333,0.260416666666667,0.265625),.UNSPECIFIED.)
CURVE()
GEOMETRIC_REPRESENTATION_ITEM()
RATIONAL_B_SPLINE_CURVE((1.,0.866025403784439,1.,0.866025403784439,1.,0.866025403784439,
1.,0.866025403784439,1.,0.866025403784439,1.,0.866025403784439,1.))
REPRESENTATION_ITEM('')
);
#203=(
BOUNDED_CURVE()
B_SPLINE_CURVE(2,(#25220,#25221,#25222,#25223,#25224,#25225,#25226,#25227,
#25228,#25229,#25230,#25231,#25232),.UNSPECIFIED.,.F.,.F.)
B_SPLINE_CURVE_WITH_KNOTS((3,2,2,2,2,2,3),(0.234375,0.239583333333333,0.244791666666667,
0.25,0.255208333333333,0.260416666666667,0.265625),.UNSPECIFIED.)
CURVE()
GEOMETRIC_REPRESENTATION_ITEM()
RATIONAL_B_SPLINE_CURVE((1.,0.866025403784439,1.,0.866025403784439,1.,0.866025403784439,
1.,0.866025403784439,1.,0.866025403784439,1.,0.866025403784439,1.))
REPRESENTATION_ITEM('')
);
#204=(
BOUNDED_CURVE()
B_SPLINE_CURVE(2,(#25237,#25238,#25239,#25240,#25241,#25242,#25243,#25244,
#25245,#25246,#25247,#25248,#25249),.UNSPECIFIED.,.F.,.F.)
B_SPLINE_CURVE_WITH_KNOTS((3,2,2,2,2,2,3),(0.265625,0.270833333333333,0.276041666666667,
0.28125,0.286458333333333,0.291666666666667,0.296875),.UNSPECIFIED.)
CURVE()
GEOMETRIC_REPRESENTATION_ITEM()
RATIONAL_B_SPLINE_CURVE((1.,0.866025403784439,1.,0.866025403784439,1.,0.866025403784439,
1.,0.866025403784439,1.,0.866025403784439,1.,0.866025403784439,1.))
REPRESENTATION_ITEM('')
);
#205=(
BOUNDED_CURVE()
B_SPLINE_CURVE(2,(#25250,#25251,#25252,#25253,#25254,#25255,#25256,#25257,
#25258,#25259,#25260,#25261,#25262),.UNSPECIFIED.,.F.,.F.)
B_SPLINE_CURVE_WITH_KNOTS((3,2,2,2,2,2,3),(0.265625,0.270833333333333,0.276041666666667,
0.28125,0.286458333333333,0.291666666666667,0.296875),.UNSPECIFIED.)
CURVE()
GEOMETRIC_REPRESENTATION_ITEM()
RATIONAL_B_SPLINE_CURVE((1.,0.866025403784439,1.,0.866025403784439,1.,0.866025403784439,
1.,0.866025403784439,1.,0.866025403784439,1.,0.866025403784439,1.))
REPRESENTATION_ITEM('')
);
#206=(
BOUNDED_CURVE()
B_SPLINE_CURVE(2,(#25267,#25268,#25269,#25270,#25271,#25272,#25273,#25274,
#25275,#25276,#25277,#25278,#25279),.UNSPECIFIED.,.F.,.F.)
B_SPLINE_CURVE_WITH_KNOTS((3,2,2,2,2,2,3),(0.296875,0.302083333333333,0.307291666666667,
0.3125,0.317708333333333,0.322916666666667,0.328125),.UNSPECIFIED.)
CURVE()
GEOMETRIC_REPRESENTATION_ITEM()
RATIONAL_B_SPLINE_CURVE((1.,0.866025403784439,1.,0.866025403784439,1.,0.866025403784439,
1.,0.866025403784439,1.,0.866025403784439,1.,0.866025403784439,1.))
REPRESENTATION_ITEM('')
);
#207=(
BOUNDED_CURVE()
B_SPLINE_CURVE(2,(#25280,#25281,#25282,#25283,#25284,#25285,#25286,#25287,
#25288,#25289,#25290,#25291,#25292),.UNSPECIFIED.,.F.,.F.)
B_SPLINE_CURVE_WITH_KNOTS((3,2,2,2,2,2,3),(0.296875,0.302083333333333,0.307291666666667,
0.3125,0.317708333333333,0.322916666666667,0.328125),.UNSPECIFIED.)
CURVE()
GEOMETRIC_REPRESENTATION_ITEM()
RATIONAL_B_SPLINE_CURVE((1.,0.866025403784439,1.,0.866025403784439,1.,0.866025403784439,
1.,0.866025403784439,1.,0.866025403784439,1.,0.866025403784439,1.))
REPRESENTATION_ITEM('')
);
#208=(
BOUNDED_CURVE()
B_SPLINE_CURVE(2,(#25297,#25298,#25299,#25300,#25301,#25302,#25303,#25304,
#25305,#25306,#25307,#25308,#25309),.UNSPECIFIED.,.F.,.F.)
B_SPLINE_CURVE_WITH_KNOTS((3,2,2,2,2,2,3),(0.328125,0.333333333333333,0.338541666666667,
0.34375,0.348958333333333,0.354166666666667,0.359375),.UNSPECIFIED.)
CURVE()
GEOMETRIC_REPRESENTATION_ITEM()
RATIONAL_B_SPLINE_CURVE((1.,0.866025403784439,1.,0.866025403784439,1.,0.866025403784439,
1.,0.866025403784439,1.,0.866025403784439,1.,0.866025403784439,1.))
REPRESENTATION_ITEM('')
);
#209=(
BOUNDED_CURVE()
B_SPLINE_CURVE(2,(#25310,#25311,#25312,#25313,#25314,#25315,#25316,#25317,
#25318,#25319,#25320,#25321,#25322),.UNSPECIFIED.,.F.,.F.)
B_SPLINE_CURVE_WITH_KNOTS((3,2,2,2,2,2,3),(0.328125,0.333333333333333,0.338541666666667,
0.34375,0.348958333333333,0.354166666666667,0.359375),.UNSPECIFIED.)
CURVE()
GEOMETRIC_REPRESENTATION_ITEM()
RATIONAL_B_SPLINE_CURVE((1.,0.866025403784439,1.,0.866025403784439,1.,0.866025403784439,
1.,0.866025403784439,1.,0.866025403784439,1.,0.866025403784439,1.))
REPRESENTATION_ITEM('')
);
#210=(
BOUNDED_CURVE()
B_SPLINE_CURVE(2,(#25327,#25328,#25329,#25330,#25331,#25332,#25333,#25334,
#25335,#25336,#25337,#25338,#25339),.UNSPECIFIED.,.F.,.F.)
B_SPLINE_CURVE_WITH_KNOTS((3,2,2,2,2,2,3),(0.359375,0.364583333333333,0.369791666666667,
0.375,0.380208333333333,0.385416666666667,0.390625),.UNSPECIFIED.)
CURVE()
GEOMETRIC_REPRESENTATION_ITEM()
RATIONAL_B_SPLINE_CURVE((1.,0.866025403784439,1.,0.866025403784439,1.,0.866025403784439,
1.,0.866025403784439,1.,0.866025403784439,1.,0.866025403784439,1.))
REPRESENTATION_ITEM('')
);
#211=(
BOUNDED_CURVE()
B_SPLINE_CURVE(2,(#25340,#25341,#25342,#25343,#25344,#25345,#25346,#25347,
#25348,#25349,#25350,#25351,#25352),.UNSPECIFIED.,.F.,.F.)
B_SPLINE_CURVE_WITH_KNOTS((3,2,2,2,2,2,3),(0.359375,0.364583333333333,0.369791666666667,
0.375,0.380208333333333,0.385416666666667,0.390625),.UNSPECIFIED.)
CURVE()
GEOMETRIC_REPRESENTATION_ITEM()
RATIONAL_B_SPLINE_CURVE((1.,0.866025403784439,1.,0.866025403784439,1.,0.866025403784439,
1.,0.866025403784439,1.,0.866025403784439,1.,0.866025403784439,1.))
REPRESENTATION_ITEM('')
);
#212=(
BOUNDED_CURVE()
B_SPLINE_CURVE(2,(#25357,#25358,#25359,#25360,#25361,#25362,#25363,#25364,
#25365,#25366,#25367,#25368,#25369),.UNSPECIFIED.,.F.,.F.)
B_SPLINE_CURVE_WITH_KNOTS((3,2,2,2,2,2,3),(0.390625,0.395833333333333,0.401041666666667,
0.40625,0.411458333333333,0.416666666666667,0.421875),.UNSPECIFIED.)
CURVE()
GEOMETRIC_REPRESENTATION_ITEM()
RATIONAL_B_SPLINE_CURVE((1.,0.866025403784439,1.,0.866025403784439,1.,0.866025403784439,
1.,0.866025403784439,1.,0.866025403784439,1.,0.866025403784439,1.))
REPRESENTATION_ITEM('')
);
#213=(
BOUNDED_CURVE()
B_SPLINE_CURVE(2,(#25370,#25371,#25372,#25373,#25374,#25375,#25376,#25377,
#25378,#25379,#25380,#25381,#25382),.UNSPECIFIED.,.F.,.F.)
B_SPLINE_CURVE_WITH_KNOTS((3,2,2,2,2,2,3),(0.390625,0.395833333333333,0.401041666666667,
0.40625,0.411458333333333,0.416666666666667,0.421875),.UNSPECIFIED.)
CURVE()
GEOMETRIC_REPRESENTATION_ITEM()
RATIONAL_B_SPLINE_CURVE((1.,0.866025403784439,1.,0.866025403784439,1.,0.866025403784439,
1.,0.866025403784439,1.,0.866025403784439,1.,0.866025403784439,1.))
REPRESENTATION_ITEM('')
);
#214=(
BOUNDED_CURVE()
B_SPLINE_CURVE(2,(#25387,#25388,#25389,#25390,#25391,#25392,#25393,#25394,
#25395,#25396,#25397,#25398,#25399),.UNSPECIFIED.,.F.,.F.)
B_SPLINE_CURVE_WITH_KNOTS((3,2,2,2,2,2,3),(0.421875,0.427083333333333,0.432291666666667,
0.4375,0.442708333333333,0.447916666666667,0.453125),.UNSPECIFIED.)
CURVE()
GEOMETRIC_REPRESENTATION_ITEM()
RATIONAL_B_SPLINE_CURVE((1.,0.866025403784439,1.,0.866025403784439,1.,0.866025403784439,
1.,0.866025403784439,1.,0.866025403784439,1.,0.866025403784439,1.))
REPRESENTATION_ITEM('')
);
#215=(
BOUNDED_CURVE()
B_SPLINE_CURVE(2,(#25400,#25401,#25402,#25403,#25404,#25405,#25406,#25407,
#25408,#25409,#25410,#25411,#25412),.UNSPECIFIED.,.F.,.F.)
B_SPLINE_CURVE_WITH_KNOTS((3,2,2,2,2,2,3),(0.421875,0.427083333333333,0.432291666666667,
0.4375,0.442708333333333,0.447916666666667,0.453125),.UNSPECIFIED.)
CURVE()
GEOMETRIC_REPRESENTATION_ITEM()
RATIONAL_B_SPLINE_CURVE((1.,0.866025403784439,1.,0.866025403784439,1.,0.866025403784439,
1.,0.866025403784439,1.,0.866025403784439,1.,0.866025403784439,1.))
REPRESENTATION_ITEM('')
);
#216=(
BOUNDED_CURVE()
B_SPLINE_CURVE(2,(#25417,#25418,#25419,#25420,#25421,#25422,#25423,#25424,
#25425,#25426,#25427,#25428,#25429),.UNSPECIFIED.,.F.,.F.)
B_SPLINE_CURVE_WITH_KNOTS((3,2,2,2,2,2,3),(0.453125,0.458333333333333,0.463541666666667,
0.46875,0.473958333333333,0.479166666666667,0.484375),.UNSPECIFIED.)
CURVE()
GEOMETRIC_REPRESENTATION_ITEM()
RATIONAL_B_SPLINE_CURVE((1.,0.866025403784439,1.,0.866025403784439,1.,0.866025403784439,
1.,0.866025403784439,1.,0.866025403784439,1.,0.866025403784439,1.))
REPRESENTATION_ITEM('')
);
#217=(
BOUNDED_CURVE()
B_SPLINE_CURVE(2,(#25430,#25431,#25432,#25433,#25434,#25435,#25436,#25437,
#25438,#25439,#25440,#25441,#25442),.UNSPECIFIED.,.F.,.F.)
B_SPLINE_CURVE_WITH_KNOTS((3,2,2,2,2,2,3),(0.453125,0.458333333333333,0.463541666666667,
0.46875,0.473958333333333,0.479166666666667,0.484375),.UNSPECIFIED.)
CURVE()
GEOMETRIC_REPRESENTATION_ITEM()
RATIONAL_B_SPLINE_CURVE((1.,0.866025403784439,1.,0.866025403784439,1.,0.866025403784439,
1.,0.866025403784439,1.,0.866025403784439,1.,0.866025403784439,1.))
REPRESENTATION_ITEM('')
);
#218=(
BOUNDED_CURVE()
B_SPLINE_CURVE(2,(#25447,#25448,#25449,#25450,#25451,#25452,#25453,#25454,
#25455,#25456,#25457,#25458,#25459),.UNSPECIFIED.,.F.,.F.)
B_SPLINE_CURVE_WITH_KNOTS((3,2,2,2,2,2,3),(0.484375,0.489583333333333,0.494791666666667,
0.5,0.505208333333333,0.510416666666667,0.515625),.UNSPECIFIED.)
CURVE()
GEOMETRIC_REPRESENTATION_ITEM()
RATIONAL_B_SPLINE_CURVE((1.,0.866025403784439,1.,0.866025403784439,1.,0.866025403784439,
1.,0.866025403784439,1.,0.866025403784439,1.,0.866025403784439,1.))
REPRESENTATION_ITEM('')
);
#219=(
BOUNDED_CURVE()
B_SPLINE_CURVE(2,(#25460,#25461,#25462,#25463,#25464,#25465,#25466,#25467,
#25468,#25469,#25470,#25471,#25472),.UNSPECIFIED.,.F.,.F.)
B_SPLINE_CURVE_WITH_KNOTS((3,2,2,2,2,2,3),(0.484375,0.489583333333333,0.494791666666667,
0.5,0.505208333333333,0.510416666666667,0.515625),.UNSPECIFIED.)
CURVE()
GEOMETRIC_REPRESENTATION_ITEM()
RATIONAL_B_SPLINE_CURVE((1.,0.866025403784439,1.,0.866025403784439,1.,0.866025403784439,
1.,0.866025403784439,1.,0.866025403784439,1.,0.866025403784439,1.))
REPRESENTATION_ITEM('')
);
#220=(
BOUNDED_CURVE()
B_SPLINE_CURVE(2,(#25477,#25478,#25479,#25480,#25481,#25482,#25483,#25484,
#25485,#25486,#25487,#25488,#25489),.UNSPECIFIED.,.F.,.F.)
B_SPLINE_CURVE_WITH_KNOTS((3,2,2,2,2,2,3),(0.515625,0.520833333333333,0.526041666666667,
0.53125,0.536458333333333,0.541666666666667,0.546875),.UNSPECIFIED.)
CURVE()
GEOMETRIC_REPRESENTATION_ITEM()
RATIONAL_B_SPLINE_CURVE((1.,0.866025403784439,1.,0.866025403784439,1.,0.866025403784439,
1.,0.866025403784439,1.,0.866025403784439,1.,0.866025403784439,1.))
REPRESENTATION_ITEM('')
);
#221=(
BOUNDED_CURVE()
B_SPLINE_CURVE(2,(#25490,#25491,#25492,#25493,#25494,#25495,#25496,#25497,
#25498,#25499,#25500,#25501,#25502),.UNSPECIFIED.,.F.,.F.)
B_SPLINE_CURVE_WITH_KNOTS((3,2,2,2,2,2,3),(0.515625,0.520833333333333,0.526041666666667,
0.53125,0.536458333333333,0.541666666666667,0.546875),.UNSPECIFIED.)
CURVE()
GEOMETRIC_REPRESENTATION_ITEM()
RATIONAL_B_SPLINE_CURVE((1.,0.866025403784439,1.,0.866025403784439,1.,0.866025403784439,
1.,0.866025403784439,1.,0.866025403784439,1.,0.866025403784439,1.))
REPRESENTATION_ITEM('')
);
#222=(
BOUNDED_CURVE()
B_SPLINE_CURVE(2,(#25507,#25508,#25509,#25510,#25511,#25512,#25513,#25514,
#25515,#25516,#25517,#25518,#25519),.UNSPECIFIED.,.F.,.F.)
B_SPLINE_CURVE_WITH_KNOTS((3,2,2,2,2,2,3),(0.546875,0.552083333333333,0.557291666666667,
0.5625,0.567708333333333,0.572916666666667,0.578125),.UNSPECIFIED.)
CURVE()
GEOMETRIC_REPRESENTATION_ITEM()
RATIONAL_B_SPLINE_CURVE((1.,0.866025403784439,1.,0.866025403784439,1.,0.866025403784439,
1.,0.866025403784439,1.,0.866025403784439,1.,0.866025403784439,1.))
REPRESENTATION_ITEM('')
);
#223=(
BOUNDED_CURVE()
B_SPLINE_CURVE(2,(#25520,#25521,#25522,#25523,#25524,#25525,#25526,#25527,
#25528,#25529,#25530,#25531,#25532),.UNSPECIFIED.,.F.,.F.)
B_SPLINE_CURVE_WITH_KNOTS((3,2,2,2,2,2,3),(0.546875,0.552083333333333,0.557291666666667,
0.5625,0.567708333333333,0.572916666666667,0.578125),.UNSPECIFIED.)
CURVE()
GEOMETRIC_REPRESENTATION_ITEM()
RATIONAL_B_SPLINE_CURVE((1.,0.866025403784439,1.,0.866025403784439,1.,0.866025403784439,
1.,0.866025403784439,1.,0.866025403784439,1.,0.866025403784439,1.))
REPRESENTATION_ITEM('')
);
#224=(
BOUNDED_CURVE()
B_SPLINE_CURVE(2,(#25537,#25538,#25539,#25540,#25541,#25542,#25543,#25544,
#25545,#25546,#25547,#25548,#25549),.UNSPECIFIED.,.F.,.F.)
B_SPLINE_CURVE_WITH_KNOTS((3,2,2,2,2,2,3),(0.578125,0.583333333333333,0.588541666666667,
0.59375,0.598958333333333,0.604166666666667,0.609375),.UNSPECIFIED.)
CURVE()
GEOMETRIC_REPRESENTATION_ITEM()
RATIONAL_B_SPLINE_CURVE((1.,0.866025403784439,1.,0.866025403784439,1.,0.866025403784439,
1.,0.866025403784439,1.,0.866025403784439,1.,0.866025403784439,1.))
REPRESENTATION_ITEM('')
);
#225=(
BOUNDED_CURVE()
B_SPLINE_CURVE(2,(#25550,#25551,#25552,#25553,#25554,#25555,#25556,#25557,
#25558,#25559,#25560,#25561,#25562),.UNSPECIFIED.,.F.,.F.)
B_SPLINE_CURVE_WITH_KNOTS((3,2,2,2,2,2,3),(0.578125,0.583333333333333,0.588541666666667,
0.59375,0.598958333333333,0.604166666666667,0.609375),.UNSPECIFIED.)
CURVE()
GEOMETRIC_REPRESENTATION_ITEM()
RATIONAL_B_SPLINE_CURVE((1.,0.866025403784439,1.,0.866025403784439,1.,0.866025403784439,
1.,0.866025403784439,1.,0.866025403784439,1.,0.866025403784439,1.))
REPRESENTATION_ITEM('')
);
#226=(
BOUNDED_CURVE()
B_SPLINE_CURVE(2,(#25567,#25568,#25569,#25570,#25571,#25572,#25573,#25574,
#25575,#25576,#25577,#25578,#25579),.UNSPECIFIED.,.F.,.F.)
B_SPLINE_CURVE_WITH_KNOTS((3,2,2,2,2,2,3),(0.609375,0.614583333333333,0.619791666666667,
0.625,0.630208333333333,0.635416666666667,0.640625),.UNSPECIFIED.)
CURVE()
GEOMETRIC_REPRESENTATION_ITEM()
RATIONAL_B_SPLINE_CURVE((1.,0.866025403784439,1.,0.866025403784439,1.,0.866025403784439,
1.,0.866025403784439,1.,0.866025403784439,1.,0.866025403784439,1.))
REPRESENTATION_ITEM('')
);
#227=(
BOUNDED_CURVE()
B_SPLINE_CURVE(2,(#25580,#25581,#25582,#25583,#25584,#25585,#25586,#25587,
#25588,#25589,#25590,#25591,#25592),.UNSPECIFIED.,.F.,.F.)
B_SPLINE_CURVE_WITH_KNOTS((3,2,2,2,2,2,3),(0.609375,0.614583333333333,0.619791666666667,
0.625,0.630208333333333,0.635416666666667,0.640625),.UNSPECIFIED.)
CURVE()
GEOMETRIC_REPRESENTATION_ITEM()
RATIONAL_B_SPLINE_CURVE((1.,0.866025403784439,1.,0.866025403784439,1.,0.866025403784439,
1.,0.866025403784439,1.,0.866025403784439,1.,0.866025403784439,1.))
REPRESENTATION_ITEM('')
);
#228=(
BOUNDED_CURVE()
B_SPLINE_CURVE(2,(#25597,#25598,#25599,#25600,#25601,#25602,#25603,#25604,
#25605,#25606,#25607,#25608,#25609),.UNSPECIFIED.,.F.,.F.)
B_SPLINE_CURVE_WITH_KNOTS((3,2,2,2,2,2,3),(0.640625,0.645833333333333,0.651041666666667,
0.65625,0.661458333333333,0.666666666666667,0.671875),.UNSPECIFIED.)
CURVE()
GEOMETRIC_REPRESENTATION_ITEM()
RATIONAL_B_SPLINE_CURVE((1.,0.866025403784439,1.,0.866025403784439,1.,0.866025403784439,
1.,0.866025403784439,1.,0.866025403784439,1.,0.866025403784439,1.))
REPRESENTATION_ITEM('')
);
#229=(
BOUNDED_CURVE()
B_SPLINE_CURVE(2,(#25610,#25611,#25612,#25613,#25614,#25615,#25616,#25617,
#25618,#25619,#25620,#25621,#25622),.UNSPECIFIED.,.F.,.F.)
B_SPLINE_CURVE_WITH_KNOTS((3,2,2,2,2,2,3),(0.640625,0.645833333333333,0.651041666666667,
0.65625,0.661458333333333,0.666666666666667,0.671875),.UNSPECIFIED.)
CURVE()
GEOMETRIC_REPRESENTATION_ITEM()
RATIONAL_B_SPLINE_CURVE((1.,0.866025403784439,1.,0.866025403784439,1.,0.866025403784439,
1.,0.866025403784439,1.,0.866025403784439,1.,0.866025403784439,1.))
REPRESENTATION_ITEM('')
);
#230=(
BOUNDED_CURVE()
B_SPLINE_CURVE(2,(#25627,#25628,#25629,#25630,#25631,#25632,#25633,#25634,
#25635,#25636,#25637,#25638,#25639),.UNSPECIFIED.,.F.,.F.)
B_SPLINE_CURVE_WITH_KNOTS((3,2,2,2,2,2,3),(0.671875,0.677083333333333,0.682291666666667,
0.6875,0.692708333333333,0.697916666666667,0.703125),.UNSPECIFIED.)
CURVE()
GEOMETRIC_REPRESENTATION_ITEM()
RATIONAL_B_SPLINE_CURVE((1.,0.866025403784439,1.,0.866025403784439,1.,0.866025403784439,
1.,0.866025403784439,1.,0.866025403784439,1.,0.866025403784439,1.))
REPRESENTATION_ITEM('')
);
#231=(
BOUNDED_CURVE()
B_SPLINE_CURVE(2,(#25640,#25641,#25642,#25643,#25644,#25645,#25646,#25647,
#25648,#25649,#25650,#25651,#25652),.UNSPECIFIED.,.F.,.F.)
B_SPLINE_CURVE_WITH_KNOTS((3,2,2,2,2,2,3),(0.671875,0.677083333333333,0.682291666666667,
0.6875,0.692708333333333,0.697916666666667,0.703125),.UNSPECIFIED.)
CURVE()
GEOMETRIC_REPRESENTATION_ITEM()
RATIONAL_B_SPLINE_CURVE((1.,0.866025403784439,1.,0.866025403784439,1.,0.866025403784439,
1.,0.866025403784439,1.,0.866025403784439,1.,0.866025403784439,1.))
REPRESENTATION_ITEM('')
);
#232=(
BOUNDED_CURVE()
B_SPLINE_CURVE(2,(#25657,#25658,#25659,#25660,#25661,#25662,#25663,#25664,
#25665,#25666,#25667,#25668,#25669),.UNSPECIFIED.,.F.,.F.)
B_SPLINE_CURVE_WITH_KNOTS((3,2,2,2,2,2,3),(0.703125,0.708333333333333,0.713541666666667,
0.71875,0.723958333333333,0.729166666666667,0.734375),.UNSPECIFIED.)
CURVE()
GEOMETRIC_REPRESENTATION_ITEM()
RATIONAL_B_SPLINE_CURVE((1.,0.866025403784439,1.,0.866025403784439,1.,0.866025403784439,
1.,0.866025403784439,1.,0.866025403784439,1.,0.866025403784439,1.))
REPRESENTATION_ITEM('')
);
#233=(
BOUNDED_CURVE()
B_SPLINE_CURVE(2,(#25670,#25671,#25672,#25673,#25674,#25675,#25676,#25677,
#25678,#25679,#25680,#25681,#25682),.UNSPECIFIED.,.F.,.F.)
B_SPLINE_CURVE_WITH_KNOTS((3,2,2,2,2,2,3),(0.703125,0.708333333333333,0.713541666666667,
0.71875,0.723958333333333,0.729166666666667,0.734375),.UNSPECIFIED.)
CURVE()
GEOMETRIC_REPRESENTATION_ITEM()
RATIONAL_B_SPLINE_CURVE((1.,0.866025403784439,1.,0.866025403784439,1.,0.866025403784439,
1.,0.866025403784439,1.,0.866025403784439,1.,0.866025403784439,1.))
REPRESENTATION_ITEM('')
);
#234=(
BOUNDED_CURVE()
B_SPLINE_CURVE(2,(#25688,#25689,#25690,#25691,#25692),.UNSPECIFIED.,.F.,
 .F.)
B_SPLINE_CURVE_WITH_KNOTS((3,2,3),(0.765625,0.770833333333333,0.771318117457215),
 .UNSPECIFIED.)
CURVE()
GEOMETRIC_REPRESENTATION_ITEM()
RATIONAL_B_SPLINE_CURVE((1.,0.866025403784439,1.,0.987529838608244,0.977381086342234))
REPRESENTATION_ITEM('')
);
#235=(
BOUNDED_CURVE()
B_SPLINE_CURVE(2,(#25695,#25696,#25697,#25698,#25699),.UNSPECIFIED.,.F.,
 .F.)
B_SPLINE_CURVE_WITH_KNOTS((3,2,3),(0.765625,0.770833333333333,0.775106737579528),
 .UNSPECIFIED.)
CURVE()
GEOMETRIC_REPRESENTATION_ITEM()
RATIONAL_B_SPLINE_CURVE((1.,0.866025403784439,1.,0.890074699196848,0.960535413324785))
REPRESENTATION_ITEM('')
);
#236=(
BOUNDED_CURVE()
B_SPLINE_CURVE(2,(#28344,#28345,#28346,#28347,#28348,#28349,#28350,#28351,
#28352,#28353,#28354,#28355,#28356),.UNSPECIFIED.,.F.,.F.)
B_SPLINE_CURVE_WITH_KNOTS((3,2,2,2,2,2,3),(0.734375,0.739583333333333,0.744791666666667,
0.75,0.755208333333333,0.760416666666667,0.765625),.UNSPECIFIED.)
CURVE()
GEOMETRIC_REPRESENTATION_ITEM()
RATIONAL_B_SPLINE_CURVE((1.,0.866025403784439,1.,0.866025403784439,1.,0.866025403784439,
1.,0.866025403784439,1.,0.866025403784439,1.,0.866025403784439,1.))
REPRESENTATION_ITEM('')
);
#237=(
BOUNDED_CURVE()
B_SPLINE_CURVE(2,(#28357,#28358,#28359,#28360,#28361,#28362,#28363,#28364,
#28365,#28366,#28367,#28368,#28369),.UNSPECIFIED.,.F.,.F.)
B_SPLINE_CURVE_WITH_KNOTS((3,2,2,2,2,2,3),(0.734375,0.739583333333333,0.744791666666667,
0.75,0.755208333333333,0.760416666666667,0.765625),.UNSPECIFIED.)
CURVE()
GEOMETRIC_REPRESENTATION_ITEM()
RATIONAL_B_SPLINE_CURVE((1.,0.866025403784439,1.,0.866025403784439,1.,0.866025403784439,
1.,0.866025403784439,1.,0.866025403784439,1.,0.866025403784439,1.))
REPRESENTATION_ITEM('')
);
#238=(
BOUNDED_CURVE()
B_SPLINE_CURVE(2,(#33393,#33394,#33395),.UNSPECIFIED.,.F.,.F.)
B_SPLINE_CURVE_WITH_KNOTS((3,3),(0.0421543904155743,0.059561882542862),
 .UNSPECIFIED.)
CURVE()
GEOMETRIC_REPRESENTATION_ITEM()
RATIONAL_B_SPLINE_CURVE((1.21505376344088,1.25768410333319,1.29885057471263))
REPRESENTATION_ITEM('')
);
#239=(
BOUNDED_CURVE()
B_SPLINE_CURVE(2,(#33398,#33399,#33400),.UNSPECIFIED.,.F.,.F.)
B_SPLINE_CURVE_WITH_KNOTS((3,3),(-0.162076637737085,-0.10981765032222),
 .UNSPECIFIED.)
CURVE()
GEOMETRIC_REPRESENTATION_ITEM()
RATIONAL_B_SPLINE_CURVE((1.22222222222222,1.19527460940787,1.16260162601569))
REPRESENTATION_ITEM('')
);
#240=(
BOUNDED_CURVE()
B_SPLINE_CURVE(2,(#33434,#33435,#33436),.UNSPECIFIED.,.F.,.F.)
B_SPLINE_CURVE_WITH_KNOTS((3,3),(0.109817650322217,0.162076637737086),
 .UNSPECIFIED.)
CURVE()
GEOMETRIC_REPRESENTATION_ITEM()
RATIONAL_B_SPLINE_CURVE((1.16260162601569,1.19527460940787,1.22222222222222))
REPRESENTATION_ITEM('')
);
#241=(
BOUNDED_CURVE()
B_SPLINE_CURVE(2,(#33439,#33440,#33441),.UNSPECIFIED.,.F.,.F.)
B_SPLINE_CURVE_WITH_KNOTS((3,3),(-0.0595618825429998,-0.0421543904157002),
 .UNSPECIFIED.)
CURVE()
GEOMETRIC_REPRESENTATION_ITEM()
RATIONAL_B_SPLINE_CURVE((1.29885057471333,1.25768410333386,1.21505376344153))
REPRESENTATION_ITEM('')
);
#242=(
BOUNDED_CURVE()
B_SPLINE_CURVE(2,(#34217,#34218,#34219),.UNSPECIFIED.,.F.,.F.)
B_SPLINE_CURVE_WITH_KNOTS((3,3),(0.536094506482407,0.589144372850599),
 .UNSPECIFIED.)
CURVE()
GEOMETRIC_REPRESENTATION_ITEM()
RATIONAL_B_SPLINE_CURVE((1.0242816296211,1.02311336089471,1.02147610370002))
REPRESENTATION_ITEM('')
);
#243=(
BOUNDED_CURVE()
B_SPLINE_CURVE(2,(#34223,#34224,#34225),.UNSPECIFIED.,.F.,.F.)
B_SPLINE_CURVE_WITH_KNOTS((3,3),(0.218746031477168,0.271795897845357),
 .UNSPECIFIED.)
CURVE()
GEOMETRIC_REPRESENTATION_ITEM()
RATIONAL_B_SPLINE_CURVE((1.02147610369998,1.02311336089466,1.02428162962105))
REPRESENTATION_ITEM('')
);
#244=(
BOUNDED_CURVE()
B_SPLINE_CURVE(2,(#34227,#34228,#34229),.UNSPECIFIED.,.F.,.F.)
B_SPLINE_CURVE_WITH_KNOTS((3,3),(0.536094506482406,0.589144372850588),
 .UNSPECIFIED.)
CURVE()
GEOMETRIC_REPRESENTATION_ITEM()
RATIONAL_B_SPLINE_CURVE((1.02428162962092,1.02311336089453,1.02147610369986))
REPRESENTATION_ITEM('')
);
#245=(
BOUNDED_CURVE()
B_SPLINE_CURVE(2,(#34233,#34234,#34235),.UNSPECIFIED.,.F.,.F.)
B_SPLINE_CURVE_WITH_KNOTS((3,3),(0.21874603147717,0.271795897845354),
 .UNSPECIFIED.)
CURVE()
GEOMETRIC_REPRESENTATION_ITEM()
RATIONAL_B_SPLINE_CURVE((1.02147610369991,1.02311336089458,1.02428162962097))
REPRESENTATION_ITEM('')
);
#246=(
BOUNDED_CURVE()
B_SPLINE_CURVE(2,(#34237,#34238,#34239),.UNSPECIFIED.,.F.,.F.)
B_SPLINE_CURVE_WITH_KNOTS((3,3),(0.536094506482412,0.589144372850605),
 .UNSPECIFIED.)
CURVE()
GEOMETRIC_REPRESENTATION_ITEM()
RATIONAL_B_SPLINE_CURVE((1.02428162962116,1.02311336089476,1.02147610370007))
REPRESENTATION_ITEM('')
);
#247=(
BOUNDED_CURVE()
B_SPLINE_CURVE(2,(#34243,#34244,#34245),.UNSPECIFIED.,.F.,.F.)
B_SPLINE_CURVE_WITH_KNOTS((3,3),(0.218746031477164,0.27179589784535),
 .UNSPECIFIED.)
CURVE()
GEOMETRIC_REPRESENTATION_ITEM()
RATIONAL_B_SPLINE_CURVE((1.02147610369995,1.02311336089462,1.02428162962101))
REPRESENTATION_ITEM('')
);
#248=(
BOUNDED_CURVE()
B_SPLINE_CURVE(2,(#34247,#34248,#34249),.UNSPECIFIED.,.F.,.F.)
B_SPLINE_CURVE_WITH_KNOTS((3,3),(0.536094506482389,0.589144372850566),
 .UNSPECIFIED.)
CURVE()
GEOMETRIC_REPRESENTATION_ITEM()
RATIONAL_B_SPLINE_CURVE((1.0242816296208,1.02311336089442,1.02147610369976))
REPRESENTATION_ITEM('')
);
#249=(
BOUNDED_CURVE()
B_SPLINE_CURVE(2,(#34253,#34254,#34255),.UNSPECIFIED.,.F.,.F.)
B_SPLINE_CURVE_WITH_KNOTS((3,3),(0.218746031477182,0.271795897845361),
 .UNSPECIFIED.)
CURVE()
GEOMETRIC_REPRESENTATION_ITEM()
RATIONAL_B_SPLINE_CURVE((1.02147610369979,1.02311336089445,1.02428162962083))
REPRESENTATION_ITEM('')
);
#250=(
BOUNDED_CURVE()
B_SPLINE_CURVE(2,(#34257,#34258,#34259),.UNSPECIFIED.,.F.,.F.)
B_SPLINE_CURVE_WITH_KNOTS((3,3),(0.536094506482412,0.589144372850601),
 .UNSPECIFIED.)
CURVE()
GEOMETRIC_REPRESENTATION_ITEM()
RATIONAL_B_SPLINE_CURVE((1.02428162962106,1.02311336089466,1.02147610369999))
REPRESENTATION_ITEM('')
);
#251=(
BOUNDED_CURVE()
B_SPLINE_CURVE(2,(#34263,#34264,#34265),.UNSPECIFIED.,.F.,.F.)
B_SPLINE_CURVE_WITH_KNOTS((3,3),(0.218746031477185,0.271795897845363),
 .UNSPECIFIED.)
CURVE()
GEOMETRIC_REPRESENTATION_ITEM()
RATIONAL_B_SPLINE_CURVE((1.02147610369979,1.02311336089445,1.02428162962084))
REPRESENTATION_ITEM('')
);
#252=(
BOUNDED_CURVE()
B_SPLINE_CURVE(2,(#34267,#34268,#34269),.UNSPECIFIED.,.F.,.F.)
B_SPLINE_CURVE_WITH_KNOTS((3,3),(0.536094506482394,0.589144372850572),
 .UNSPECIFIED.)
CURVE()
GEOMETRIC_REPRESENTATION_ITEM()
RATIONAL_B_SPLINE_CURVE((1.02428162962082,1.02311336089444,1.02147610369978))
REPRESENTATION_ITEM('')
);
#253=(
BOUNDED_CURVE()
B_SPLINE_CURVE(2,(#34273,#34274,#34275),.UNSPECIFIED.,.F.,.F.)
B_SPLINE_CURVE_WITH_KNOTS((3,3),(0.21874603147717,0.271795897845349),
 .UNSPECIFIED.)
CURVE()
GEOMETRIC_REPRESENTATION_ITEM()
RATIONAL_B_SPLINE_CURVE((1.02147610369983,1.0231133608945,1.02428162962088))
REPRESENTATION_ITEM('')
);
#254=(
BOUNDED_CURVE()
B_SPLINE_CURVE(2,(#34277,#34278,#34279),.UNSPECIFIED.,.F.,.F.)
B_SPLINE_CURVE_WITH_KNOTS((3,3),(0.536094506482412,0.589144372850599),
 .UNSPECIFIED.)
CURVE()
GEOMETRIC_REPRESENTATION_ITEM()
RATIONAL_B_SPLINE_CURVE((1.02428162962104,1.02311336089465,1.02147610369997))
REPRESENTATION_ITEM('')
);
#255=(
BOUNDED_CURVE()
B_SPLINE_CURVE(2,(#34283,#34284,#34285),.UNSPECIFIED.,.F.,.F.)
B_SPLINE_CURVE_WITH_KNOTS((3,3),(0.218746031477174,0.271795897845355),
 .UNSPECIFIED.)
CURVE()
GEOMETRIC_REPRESENTATION_ITEM()
RATIONAL_B_SPLINE_CURVE((1.02147610369982,1.02311336089449,1.02428162962087))
REPRESENTATION_ITEM('')
);
#256=(
BOUNDED_CURVE()
B_SPLINE_CURVE(2,(#34287,#34288,#34289),.UNSPECIFIED.,.F.,.F.)
B_SPLINE_CURVE_WITH_KNOTS((3,3),(0.536094506482407,0.589144372850592),
 .UNSPECIFIED.)
CURVE()
GEOMETRIC_REPRESENTATION_ITEM()
RATIONAL_B_SPLINE_CURVE((1.02428162962099,1.0231133608946,1.02147610369992))
REPRESENTATION_ITEM('')
);
#257=(
BOUNDED_CURVE()
B_SPLINE_CURVE(2,(#34293,#34294,#34295),.UNSPECIFIED.,.F.,.F.)
B_SPLINE_CURVE_WITH_KNOTS((3,3),(0.218746031477156,0.271795897845345),
 .UNSPECIFIED.)
CURVE()
GEOMETRIC_REPRESENTATION_ITEM()
RATIONAL_B_SPLINE_CURVE((1.02147610369998,1.02311336089466,1.02428162962106))
REPRESENTATION_ITEM('')
);
#258=(
BOUNDED_CURVE()
B_SPLINE_CURVE(2,(#34297,#34298,#34299),.UNSPECIFIED.,.F.,.F.)
B_SPLINE_CURVE_WITH_KNOTS((3,3),(0.53609450648241,0.5891443728506),
 .UNSPECIFIED.)
CURVE()
GEOMETRIC_REPRESENTATION_ITEM()
RATIONAL_B_SPLINE_CURVE((1.02428162962108,1.02311336089468,1.0214761037))
REPRESENTATION_ITEM('')
);
#259=(
BOUNDED_CURVE()
B_SPLINE_CURVE(2,(#34303,#34304,#34305),.UNSPECIFIED.,.F.,.F.)
B_SPLINE_CURVE_WITH_KNOTS((3,3),(0.21874603147718,0.271795897845362),
 .UNSPECIFIED.)
CURVE()
GEOMETRIC_REPRESENTATION_ITEM()
RATIONAL_B_SPLINE_CURVE((1.02147610369984,1.02311336089451,1.02428162962089))
REPRESENTATION_ITEM('')
);
#260=(
BOUNDED_CURVE()
B_SPLINE_CURVE(2,(#34307,#34308,#34309),.UNSPECIFIED.,.F.,.F.)
B_SPLINE_CURVE_WITH_KNOTS((3,3),(0.536094506482414,0.589144372850597),
 .UNSPECIFIED.)
CURVE()
GEOMETRIC_REPRESENTATION_ITEM()
RATIONAL_B_SPLINE_CURVE((1.02428162962095,1.02311336089456,1.02147610369989))
REPRESENTATION_ITEM('')
);
#261=(
BOUNDED_CURVE()
B_SPLINE_CURVE(2,(#34313,#34314,#34315),.UNSPECIFIED.,.F.,.F.)
B_SPLINE_CURVE_WITH_KNOTS((3,3),(0.218746031477174,0.27179589784536),
 .UNSPECIFIED.)
CURVE()
GEOMETRIC_REPRESENTATION_ITEM()
RATIONAL_B_SPLINE_CURVE((1.02147610369991,1.02311336089459,1.02428162962097))
REPRESENTATION_ITEM('')
);
#262=(
BOUNDED_CURVE()
B_SPLINE_CURVE(2,(#34317,#34318,#34319),.UNSPECIFIED.,.F.,.F.)
B_SPLINE_CURVE_WITH_KNOTS((3,3),(0.536094506482426,0.589144372850614),
 .UNSPECIFIED.)
CURVE()
GEOMETRIC_REPRESENTATION_ITEM()
RATIONAL_B_SPLINE_CURVE((1.02428162962107,1.02311336089468,1.0214761037))
REPRESENTATION_ITEM('')
);
#263=(
BOUNDED_CURVE()
B_SPLINE_CURVE(2,(#34323,#34324,#34325),.UNSPECIFIED.,.F.,.F.)
B_SPLINE_CURVE_WITH_KNOTS((3,3),(0.218746031477169,0.271795897845354),
 .UNSPECIFIED.)
CURVE()
GEOMETRIC_REPRESENTATION_ITEM()
RATIONAL_B_SPLINE_CURVE((1.02147610369993,1.0231133608946,1.02428162962099))
REPRESENTATION_ITEM('')
);
#264=(
BOUNDED_CURVE()
B_SPLINE_CURVE(2,(#34327,#34328,#34329),.UNSPECIFIED.,.F.,.F.)
B_SPLINE_CURVE_WITH_KNOTS((3,3),(0.536094506482401,0.589144372850587),
 .UNSPECIFIED.)
CURVE()
GEOMETRIC_REPRESENTATION_ITEM()
RATIONAL_B_SPLINE_CURVE((1.02428162962099,1.0231133608946,1.02147610369993))
REPRESENTATION_ITEM('')
);
#265=(
BOUNDED_CURVE()
B_SPLINE_CURVE(2,(#34333,#34334,#34335),.UNSPECIFIED.,.F.,.F.)
B_SPLINE_CURVE_WITH_KNOTS((3,3),(0.218746031477173,0.271795897845356),
 .UNSPECIFIED.)
CURVE()
GEOMETRIC_REPRESENTATION_ITEM()
RATIONAL_B_SPLINE_CURVE((1.02147610369988,1.02311336089455,1.02428162962094))
REPRESENTATION_ITEM('')
);
#266=(
BOUNDED_CURVE()
B_SPLINE_CURVE(2,(#34337,#34338,#34339),.UNSPECIFIED.,.F.,.F.)
B_SPLINE_CURVE_WITH_KNOTS((3,3),(0.536094506482398,0.589144372850579),
 .UNSPECIFIED.)
CURVE()
GEOMETRIC_REPRESENTATION_ITEM()
RATIONAL_B_SPLINE_CURVE((1.0242816296209,1.02311336089451,1.02147610369984))
REPRESENTATION_ITEM('')
);
#267=(
BOUNDED_CURVE()
B_SPLINE_CURVE(2,(#34343,#34344,#34345),.UNSPECIFIED.,.F.,.F.)
B_SPLINE_CURVE_WITH_KNOTS((3,3),(0.218746031477172,0.271795897845351),
 .UNSPECIFIED.)
CURVE()
GEOMETRIC_REPRESENTATION_ITEM()
RATIONAL_B_SPLINE_CURVE((1.02147610369978,1.02311336089444,1.02428162962083))
REPRESENTATION_ITEM('')
);
#268=(
BOUNDED_CURVE()
B_SPLINE_CURVE(2,(#34347,#34348,#34349),.UNSPECIFIED.,.F.,.F.)
B_SPLINE_CURVE_WITH_KNOTS((3,3),(0.536094506482419,0.589144372850608),
 .UNSPECIFIED.)
CURVE()
GEOMETRIC_REPRESENTATION_ITEM()
RATIONAL_B_SPLINE_CURVE((1.02428162962106,1.02311336089467,1.02147610369999))
REPRESENTATION_ITEM('')
);
#269=(
BOUNDED_CURVE()
B_SPLINE_CURVE(2,(#34353,#34354,#34355),.UNSPECIFIED.,.F.,.F.)
B_SPLINE_CURVE_WITH_KNOTS((3,3),(0.218746031477166,0.271795897845348),
 .UNSPECIFIED.)
CURVE()
GEOMETRIC_REPRESENTATION_ITEM()
RATIONAL_B_SPLINE_CURVE((1.02147610369987,1.02311336089454,1.02428162962093))
REPRESENTATION_ITEM('')
);
#270=(
BOUNDED_CURVE()
B_SPLINE_CURVE(2,(#34357,#34358,#34359),.UNSPECIFIED.,.F.,.F.)
B_SPLINE_CURVE_WITH_KNOTS((3,3),(0.536094506482413,0.589144372850599),
 .UNSPECIFIED.)
CURVE()
GEOMETRIC_REPRESENTATION_ITEM()
RATIONAL_B_SPLINE_CURVE((1.02428162962102,1.02311336089463,1.02147610369995))
REPRESENTATION_ITEM('')
);
#271=(
BOUNDED_CURVE()
B_SPLINE_CURVE(2,(#34363,#34364,#34365),.UNSPECIFIED.,.F.,.F.)
B_SPLINE_CURVE_WITH_KNOTS((3,3),(0.218746031477176,0.271795897845356),
 .UNSPECIFIED.)
CURVE()
GEOMETRIC_REPRESENTATION_ITEM()
RATIONAL_B_SPLINE_CURVE((1.02147610369983,1.0231133608945,1.02428162962088))
REPRESENTATION_ITEM('')
);
#272=(
BOUNDED_CURVE()
B_SPLINE_CURVE(2,(#34367,#34368,#34369),.UNSPECIFIED.,.F.,.F.)
B_SPLINE_CURVE_WITH_KNOTS((3,3),(0.536094506482413,0.589144372850592),
 .UNSPECIFIED.)
CURVE()
GEOMETRIC_REPRESENTATION_ITEM()
RATIONAL_B_SPLINE_CURVE((1.02428162962088,1.02311336089449,1.02147610369982))
REPRESENTATION_ITEM('')
);
#273=(
BOUNDED_CURVE()
B_SPLINE_CURVE(2,(#34373,#34374,#34375),.UNSPECIFIED.,.F.,.F.)
B_SPLINE_CURVE_WITH_KNOTS((3,3),(0.218746031477187,0.27179589784537),
 .UNSPECIFIED.)
CURVE()
GEOMETRIC_REPRESENTATION_ITEM()
RATIONAL_B_SPLINE_CURVE((1.02147610369983,1.0231133608945,1.02428162962088))
REPRESENTATION_ITEM('')
);
#274=(
BOUNDED_CURVE()
B_SPLINE_CURVE(2,(#34377,#34378,#34379),.UNSPECIFIED.,.F.,.F.)
B_SPLINE_CURVE_WITH_KNOTS((3,3),(0.53609450648241,0.589144372850596),
 .UNSPECIFIED.)
CURVE()
GEOMETRIC_REPRESENTATION_ITEM()
RATIONAL_B_SPLINE_CURVE((1.02428162962098,1.02311336089459,1.02147610369992))
REPRESENTATION_ITEM('')
);
#275=(
BOUNDED_CURVE()
B_SPLINE_CURVE(2,(#34383,#34384,#34385),.UNSPECIFIED.,.F.,.F.)
B_SPLINE_CURVE_WITH_KNOTS((3,3),(0.218746031477173,0.271795897845356),
 .UNSPECIFIED.)
CURVE()
GEOMETRIC_REPRESENTATION_ITEM()
RATIONAL_B_SPLINE_CURVE((1.02147610369988,1.02311336089455,1.02428162962094))
REPRESENTATION_ITEM('')
);
#276=(
BOUNDED_CURVE()
B_SPLINE_CURVE(2,(#34387,#34388,#34389),.UNSPECIFIED.,.F.,.F.)
B_SPLINE_CURVE_WITH_KNOTS((3,3),(0.536094506482401,0.589144372850587),
 .UNSPECIFIED.)
CURVE()
GEOMETRIC_REPRESENTATION_ITEM()
RATIONAL_B_SPLINE_CURVE((1.024281629621,1.02311336089461,1.02147610369994))
REPRESENTATION_ITEM('')
);
#277=(
BOUNDED_CURVE()
B_SPLINE_CURVE(2,(#34393,#34394,#34395),.UNSPECIFIED.,.F.,.F.)
B_SPLINE_CURVE_WITH_KNOTS((3,3),(0.218746031477176,0.271795897845359),
 .UNSPECIFIED.)
CURVE()
GEOMETRIC_REPRESENTATION_ITEM()
RATIONAL_B_SPLINE_CURVE((1.02147610369987,1.02311336089454,1.02428162962092))
REPRESENTATION_ITEM('')
);
#278=(
BOUNDED_CURVE()
B_SPLINE_CURVE(2,(#34397,#34398,#34399),.UNSPECIFIED.,.F.,.F.)
B_SPLINE_CURVE_WITH_KNOTS((3,3),(0.536094506482401,0.589144372850584),
 .UNSPECIFIED.)
CURVE()
GEOMETRIC_REPRESENTATION_ITEM()
RATIONAL_B_SPLINE_CURVE((1.02428162962093,1.02311336089454,1.02147610369987))
REPRESENTATION_ITEM('')
);
#279=(
BOUNDED_CURVE()
B_SPLINE_CURVE(2,(#34403,#34404,#34405),.UNSPECIFIED.,.F.,.F.)
B_SPLINE_CURVE_WITH_KNOTS((3,3),(0.218746031477161,0.271795897845347),
 .UNSPECIFIED.)
CURVE()
GEOMETRIC_REPRESENTATION_ITEM()
RATIONAL_B_SPLINE_CURVE((1.02147610369995,1.02311336089462,1.02428162962101))
REPRESENTATION_ITEM('')
);
#280=(
BOUNDED_CURVE()
B_SPLINE_CURVE(2,(#34407,#34408,#34409),.UNSPECIFIED.,.F.,.F.)
B_SPLINE_CURVE_WITH_KNOTS((3,3),(0.536094506482406,0.589144372850593),
 .UNSPECIFIED.)
CURVE()
GEOMETRIC_REPRESENTATION_ITEM()
RATIONAL_B_SPLINE_CURVE((1.02428162962101,1.02311336089462,1.02147610369994))
REPRESENTATION_ITEM('')
);
#281=(
BOUNDED_CURVE()
B_SPLINE_CURVE(2,(#34413,#34414,#34415),.UNSPECIFIED.,.F.,.F.)
B_SPLINE_CURVE_WITH_KNOTS((3,3),(0.218746031477175,0.271795897845356),
 .UNSPECIFIED.)
CURVE()
GEOMETRIC_REPRESENTATION_ITEM()
RATIONAL_B_SPLINE_CURVE((1.02147610369983,1.0231133608945,1.02428162962088))
REPRESENTATION_ITEM('')
);
#282=(
BOUNDED_CURVE()
B_SPLINE_CURVE(2,(#34417,#34418,#34419),.UNSPECIFIED.,.F.,.F.)
B_SPLINE_CURVE_WITH_KNOTS((3,3),(0.536094506482409,0.589144372850594),
 .UNSPECIFIED.)
CURVE()
GEOMETRIC_REPRESENTATION_ITEM()
RATIONAL_B_SPLINE_CURVE((1.02428162962098,1.02311336089459,1.02147610369992))
REPRESENTATION_ITEM('')
);
#283=(
BOUNDED_CURVE()
B_SPLINE_CURVE(2,(#34423,#34424,#34425),.UNSPECIFIED.,.F.,.F.)
B_SPLINE_CURVE_WITH_KNOTS((3,3),(0.218746031477174,0.271795897845362),
 .UNSPECIFIED.)
CURVE()
GEOMETRIC_REPRESENTATION_ITEM()
RATIONAL_B_SPLINE_CURVE((1.02147610369994,1.02311336089462,1.02428162962101))
REPRESENTATION_ITEM('')
);
#284=(
BOUNDED_CURVE()
B_SPLINE_CURVE(2,(#34427,#34428,#34429),.UNSPECIFIED.,.F.,.F.)
B_SPLINE_CURVE_WITH_KNOTS((3,3),(0.536094506482415,0.589144372850602),
 .UNSPECIFIED.)
CURVE()
GEOMETRIC_REPRESENTATION_ITEM()
RATIONAL_B_SPLINE_CURVE((1.02428162962101,1.02311336089462,1.02147610369994))
REPRESENTATION_ITEM('')
);
#285=(
BOUNDED_CURVE()
B_SPLINE_CURVE(2,(#34433,#34434,#34435),.UNSPECIFIED.,.F.,.F.)
B_SPLINE_CURVE_WITH_KNOTS((3,3),(0.218746031477172,0.271795897845355),
 .UNSPECIFIED.)
CURVE()
GEOMETRIC_REPRESENTATION_ITEM()
RATIONAL_B_SPLINE_CURVE((1.02147610369986,1.02311336089453,1.02428162962092))
REPRESENTATION_ITEM('')
);
#286=(
BOUNDED_CURVE()
B_SPLINE_CURVE(2,(#34437,#34438,#34439),.UNSPECIFIED.,.F.,.F.)
B_SPLINE_CURVE_WITH_KNOTS((3,3),(0.536094506482405,0.589144372850589),
 .UNSPECIFIED.)
CURVE()
GEOMETRIC_REPRESENTATION_ITEM()
RATIONAL_B_SPLINE_CURVE((1.02428162962097,1.02311336089458,1.02147610369991))
REPRESENTATION_ITEM('')
);
#287=(
BOUNDED_CURVE()
B_SPLINE_CURVE(2,(#34443,#34444,#34445),.UNSPECIFIED.,.F.,.F.)
B_SPLINE_CURVE_WITH_KNOTS((3,3),(0.218746031477162,0.271795897845346),
 .UNSPECIFIED.)
CURVE()
GEOMETRIC_REPRESENTATION_ITEM()
RATIONAL_B_SPLINE_CURVE((1.02147610369991,1.02311336089459,1.02428162962098))
REPRESENTATION_ITEM('')
);
#288=(
BOUNDED_CURVE()
B_SPLINE_CURVE(2,(#34447,#34448,#34449),.UNSPECIFIED.,.F.,.F.)
B_SPLINE_CURVE_WITH_KNOTS((3,3),(0.536094506482411,0.589144372850603),
 .UNSPECIFIED.)
CURVE()
GEOMETRIC_REPRESENTATION_ITEM()
RATIONAL_B_SPLINE_CURVE((1.02428162962113,1.02311336089474,1.02147610370005))
REPRESENTATION_ITEM('')
);
#289=(
BOUNDED_CURVE()
B_SPLINE_CURVE(2,(#34453,#34454,#34455),.UNSPECIFIED.,.F.,.F.)
B_SPLINE_CURVE_WITH_KNOTS((3,3),(0.218746031477171,0.271795897845351),
 .UNSPECIFIED.)
CURVE()
GEOMETRIC_REPRESENTATION_ITEM()
RATIONAL_B_SPLINE_CURVE((1.02147610369981,1.02311336089448,1.02428162962086))
REPRESENTATION_ITEM('')
);
#290=(
BOUNDED_CURVE()
B_SPLINE_CURVE(2,(#34457,#34458,#34459),.UNSPECIFIED.,.F.,.F.)
B_SPLINE_CURVE_WITH_KNOTS((3,3),(0.536094506482409,0.589144372850599),
 .UNSPECIFIED.)
CURVE()
GEOMETRIC_REPRESENTATION_ITEM()
RATIONAL_B_SPLINE_CURVE((1.02428162962106,1.02311336089467,1.02147610369999))
REPRESENTATION_ITEM('')
);
#291=(
BOUNDED_CURVE()
B_SPLINE_CURVE(2,(#34463,#34464,#34465),.UNSPECIFIED.,.F.,.F.)
B_SPLINE_CURVE_WITH_KNOTS((3,3),(0.218746031477179,0.271795897845364),
 .UNSPECIFIED.)
CURVE()
GEOMETRIC_REPRESENTATION_ITEM()
RATIONAL_B_SPLINE_CURVE((1.02147610369988,1.02311336089455,1.02428162962094))
REPRESENTATION_ITEM('')
);
#292=(
BOUNDED_CURVE()
B_SPLINE_CURVE(2,(#34467,#34468,#34469),.UNSPECIFIED.,.F.,.F.)
B_SPLINE_CURVE_WITH_KNOTS((3,3),(0.536094506482416,0.589144372850601),
 .UNSPECIFIED.)
CURVE()
GEOMETRIC_REPRESENTATION_ITEM()
RATIONAL_B_SPLINE_CURVE((1.024281629621,1.02311336089461,1.02147610369993))
REPRESENTATION_ITEM('')
);
#293=(
BOUNDED_CURVE()
B_SPLINE_CURVE(2,(#34473,#34474,#34475),.UNSPECIFIED.,.F.,.F.)
B_SPLINE_CURVE_WITH_KNOTS((3,3),(0.218746031477175,0.27179589784536),
 .UNSPECIFIED.)
CURVE()
GEOMETRIC_REPRESENTATION_ITEM()
RATIONAL_B_SPLINE_CURVE((1.02147610369991,1.02311336089459,1.02428162962098))
REPRESENTATION_ITEM('')
);
#294=(
BOUNDED_CURVE()
B_SPLINE_CURVE(2,(#34477,#34478,#34479),.UNSPECIFIED.,.F.,.F.)
B_SPLINE_CURVE_WITH_KNOTS((3,3),(0.5360945064824,0.58914437285059),
 .UNSPECIFIED.)
CURVE()
GEOMETRIC_REPRESENTATION_ITEM()
RATIONAL_B_SPLINE_CURVE((1.02428162962107,1.02311336089468,1.0214761037))
REPRESENTATION_ITEM('')
);
#295=(
BOUNDED_CURVE()
B_SPLINE_CURVE(2,(#34483,#34484,#34485),.UNSPECIFIED.,.F.,.F.)
B_SPLINE_CURVE_WITH_KNOTS((3,3),(0.218746031477166,0.271795897845347),
 .UNSPECIFIED.)
CURVE()
GEOMETRIC_REPRESENTATION_ITEM()
RATIONAL_B_SPLINE_CURVE((1.02147610369984,1.0231133608945,1.02428162962089))
REPRESENTATION_ITEM('')
);
#296=(
BOUNDED_CURVE()
B_SPLINE_CURVE(2,(#34487,#34488,#34489),.UNSPECIFIED.,.F.,.F.)
B_SPLINE_CURVE_WITH_KNOTS((3,3),(0.536094506482403,0.589144372850591),
 .UNSPECIFIED.)
CURVE()
GEOMETRIC_REPRESENTATION_ITEM()
RATIONAL_B_SPLINE_CURVE((1.02428162962102,1.02311336089463,1.02147610369995))
REPRESENTATION_ITEM('')
);
#297=(
BOUNDED_CURVE()
B_SPLINE_CURVE(2,(#34493,#34494,#34495),.UNSPECIFIED.,.F.,.F.)
B_SPLINE_CURVE_WITH_KNOTS((3,3),(0.218746031477165,0.271795897845349),
 .UNSPECIFIED.)
CURVE()
GEOMETRIC_REPRESENTATION_ITEM()
RATIONAL_B_SPLINE_CURVE((1.02147610369991,1.02311336089458,1.02428162962097))
REPRESENTATION_ITEM('')
);
#298=(
BOUNDED_CURVE()
B_SPLINE_CURVE(2,(#34497,#34498,#34499),.UNSPECIFIED.,.F.,.F.)
B_SPLINE_CURVE_WITH_KNOTS((3,3),(0.536094506482402,0.589144372850584),
 .UNSPECIFIED.)
CURVE()
GEOMETRIC_REPRESENTATION_ITEM()
RATIONAL_B_SPLINE_CURVE((1.02428162962092,1.02311336089454,1.02147610369987))
REPRESENTATION_ITEM('')
);
#299=(
BOUNDED_CURVE()
B_SPLINE_CURVE(2,(#34503,#34504,#34505),.UNSPECIFIED.,.F.,.F.)
B_SPLINE_CURVE_WITH_KNOTS((3,3),(0.218746031477178,0.271795897845364),
 .UNSPECIFIED.)
CURVE()
GEOMETRIC_REPRESENTATION_ITEM()
RATIONAL_B_SPLINE_CURVE((1.02147610369991,1.02311336089458,1.02428162962097))
REPRESENTATION_ITEM('')
);
#300=(
BOUNDED_CURVE()
B_SPLINE_CURVE(2,(#34507,#34508,#34509),.UNSPECIFIED.,.F.,.F.)
B_SPLINE_CURVE_WITH_KNOTS((3,3),(0.536094506482408,0.589144372850591),
 .UNSPECIFIED.)
CURVE()
GEOMETRIC_REPRESENTATION_ITEM()
RATIONAL_B_SPLINE_CURVE((1.02428162962092,1.02311336089453,1.02147610369986))
REPRESENTATION_ITEM('')
);
#301=(
BOUNDED_CURVE()
B_SPLINE_CURVE(2,(#34513,#34514,#34515),.UNSPECIFIED.,.F.,.F.)
B_SPLINE_CURVE_WITH_KNOTS((3,3),(0.218746031477175,0.27179589784536),
 .UNSPECIFIED.)
CURVE()
GEOMETRIC_REPRESENTATION_ITEM()
RATIONAL_B_SPLINE_CURVE((1.02147610369989,1.02311336089456,1.02428162962095))
REPRESENTATION_ITEM('')
);
#302=(
BOUNDED_CURVE()
B_SPLINE_CURVE(2,(#34517,#34518,#34519),.UNSPECIFIED.,.F.,.F.)
B_SPLINE_CURVE_WITH_KNOTS((3,3),(0.536094506482411,0.589144372850602),
 .UNSPECIFIED.)
CURVE()
GEOMETRIC_REPRESENTATION_ITEM()
RATIONAL_B_SPLINE_CURVE((1.0242816296211,1.02311336089471,1.02147610370002))
REPRESENTATION_ITEM('')
);
#303=(
BOUNDED_CURVE()
B_SPLINE_CURVE(2,(#34523,#34524,#34525),.UNSPECIFIED.,.F.,.F.)
B_SPLINE_CURVE_WITH_KNOTS((3,3),(0.218746031477173,0.271795897845357),
 .UNSPECIFIED.)
CURVE()
GEOMETRIC_REPRESENTATION_ITEM()
RATIONAL_B_SPLINE_CURVE((1.0214761036999,1.02311336089457,1.02428162962096))
REPRESENTATION_ITEM('')
);
#304=(
BOUNDED_CURVE()
B_SPLINE_CURVE(2,(#34527,#34528,#34529),.UNSPECIFIED.,.F.,.F.)
B_SPLINE_CURVE_WITH_KNOTS((3,3),(0.536094506482408,0.589144372850595),
 .UNSPECIFIED.)
CURVE()
GEOMETRIC_REPRESENTATION_ITEM()
RATIONAL_B_SPLINE_CURVE((1.02428162962105,1.02311336089466,1.02147610369998))
REPRESENTATION_ITEM('')
);
#305=(
BOUNDED_CURVE()
B_SPLINE_CURVE(2,(#34533,#34534,#34535),.UNSPECIFIED.,.F.,.F.)
B_SPLINE_CURVE_WITH_KNOTS((3,3),(0.218746031477171,0.271795897845354),
 .UNSPECIFIED.)
CURVE()
GEOMETRIC_REPRESENTATION_ITEM()
RATIONAL_B_SPLINE_CURVE((1.02147610369989,1.02311336089456,1.02428162962095))
REPRESENTATION_ITEM('')
);
#306=(
BOUNDED_CURVE()
B_SPLINE_CURVE(2,(#34537,#34538,#34539),.UNSPECIFIED.,.F.,.F.)
B_SPLINE_CURVE_WITH_KNOTS((3,3),(0.536094506482412,0.5891443728506),
 .UNSPECIFIED.)
CURVE()
GEOMETRIC_REPRESENTATION_ITEM()
RATIONAL_B_SPLINE_CURVE((1.02428162962106,1.02311336089467,1.02147610369999))
REPRESENTATION_ITEM('')
);
#307=(
BOUNDED_CURVE()
B_SPLINE_CURVE(2,(#34543,#34544,#34545),.UNSPECIFIED.,.F.,.F.)
B_SPLINE_CURVE_WITH_KNOTS((3,3),(0.218746031477183,0.27179589784537),
 .UNSPECIFIED.)
CURVE()
GEOMETRIC_REPRESENTATION_ITEM()
RATIONAL_B_SPLINE_CURVE((1.02147610369993,1.02311336089461,1.024281629621))
REPRESENTATION_ITEM('')
);
#308=(
BOUNDED_CURVE()
B_SPLINE_CURVE(2,(#34547,#34548,#34549),.UNSPECIFIED.,.F.,.F.)
B_SPLINE_CURVE_WITH_KNOTS((3,3),(0.536094506482412,0.589144372850597),
 .UNSPECIFIED.)
CURVE()
GEOMETRIC_REPRESENTATION_ITEM()
RATIONAL_B_SPLINE_CURVE((1.02428162962099,1.0231133608946,1.02147610369993))
REPRESENTATION_ITEM('')
);
#309=(
BOUNDED_CURVE()
B_SPLINE_CURVE(2,(#34553,#34554,#34555),.UNSPECIFIED.,.F.,.F.)
B_SPLINE_CURVE_WITH_KNOTS((3,3),(0.218746031477163,0.271795897845347),
 .UNSPECIFIED.)
CURVE()
GEOMETRIC_REPRESENTATION_ITEM()
RATIONAL_B_SPLINE_CURVE((1.02147610369992,1.0231133608946,1.02428162962099))
REPRESENTATION_ITEM('')
);
#310=(
BOUNDED_CURVE()
B_SPLINE_CURVE(2,(#34557,#34558,#34559),.UNSPECIFIED.,.F.,.F.)
B_SPLINE_CURVE_WITH_KNOTS((3,3),(0.536094506482402,0.589144372850587),
 .UNSPECIFIED.)
CURVE()
GEOMETRIC_REPRESENTATION_ITEM()
RATIONAL_B_SPLINE_CURVE((1.02428162962094,1.02311336089455,1.02147610369988))
REPRESENTATION_ITEM('')
);
#311=(
BOUNDED_CURVE()
B_SPLINE_CURVE(2,(#34563,#34564,#34565),.UNSPECIFIED.,.F.,.F.)
B_SPLINE_CURVE_WITH_KNOTS((3,3),(0.218746031477181,0.271795897845363),
 .UNSPECIFIED.)
CURVE()
GEOMETRIC_REPRESENTATION_ITEM()
RATIONAL_B_SPLINE_CURVE((1.02147610369986,1.02311336089453,1.02428162962091))
REPRESENTATION_ITEM('')
);
#312=(
BOUNDED_CURVE()
B_SPLINE_CURVE(2,(#34567,#34568,#34569),.UNSPECIFIED.,.F.,.F.)
B_SPLINE_CURVE_WITH_KNOTS((3,3),(0.536094506482409,0.58914437285059),
 .UNSPECIFIED.)
CURVE()
GEOMETRIC_REPRESENTATION_ITEM()
RATIONAL_B_SPLINE_CURVE((1.02428162962091,1.02311336089453,1.02147610369986))
REPRESENTATION_ITEM('')
);
#313=(
BOUNDED_CURVE()
B_SPLINE_CURVE(2,(#34573,#34574,#34575),.UNSPECIFIED.,.F.,.F.)
B_SPLINE_CURVE_WITH_KNOTS((3,3),(0.218746031477169,0.271795897845353),
 .UNSPECIFIED.)
CURVE()
GEOMETRIC_REPRESENTATION_ITEM()
RATIONAL_B_SPLINE_CURVE((1.0214761036999,1.02311336089457,1.02428162962096))
REPRESENTATION_ITEM('')
);
#314=(
BOUNDED_CURVE()
B_SPLINE_CURVE(2,(#34577,#34578,#34579),.UNSPECIFIED.,.F.,.F.)
B_SPLINE_CURVE_WITH_KNOTS((3,3),(0.536094506482403,0.58914437285059),
 .UNSPECIFIED.)
CURVE()
GEOMETRIC_REPRESENTATION_ITEM()
RATIONAL_B_SPLINE_CURVE((1.02428162962102,1.02311336089462,1.02147610369995))
REPRESENTATION_ITEM('')
);
#315=(
BOUNDED_CURVE()
B_SPLINE_CURVE(2,(#34583,#34584,#34585),.UNSPECIFIED.,.F.,.F.)
B_SPLINE_CURVE_WITH_KNOTS((3,3),(0.218746031477163,0.271795897845352),
 .UNSPECIFIED.)
CURVE()
GEOMETRIC_REPRESENTATION_ITEM()
RATIONAL_B_SPLINE_CURVE((1.02147610369997,1.02311336089465,1.02428162962104))
REPRESENTATION_ITEM('')
);
#316=(
BOUNDED_CURVE()
B_SPLINE_CURVE(2,(#34587,#34588,#34589),.UNSPECIFIED.,.F.,.F.)
B_SPLINE_CURVE_WITH_KNOTS((3,3),(0.536094506482408,0.589144372850588),
 .UNSPECIFIED.)
CURVE()
GEOMETRIC_REPRESENTATION_ITEM()
RATIONAL_B_SPLINE_CURVE((1.02428162962085,1.02311336089447,1.0214761036998))
REPRESENTATION_ITEM('')
);
#317=(
BOUNDED_CURVE()
B_SPLINE_CURVE(2,(#34593,#34594,#34595),.UNSPECIFIED.,.F.,.F.)
B_SPLINE_CURVE_WITH_KNOTS((3,3),(0.218746031477151,0.271795897845338),
 .UNSPECIFIED.)
CURVE()
GEOMETRIC_REPRESENTATION_ITEM()
RATIONAL_B_SPLINE_CURVE((1.02147610369997,1.02311336089465,1.02428162962104))
REPRESENTATION_ITEM('')
);
#318=(
BOUNDED_CURVE()
B_SPLINE_CURVE(2,(#34597,#34598,#34599),.UNSPECIFIED.,.F.,.F.)
B_SPLINE_CURVE_WITH_KNOTS((3,3),(0.536094506482401,0.589144372850584),
 .UNSPECIFIED.)
CURVE()
GEOMETRIC_REPRESENTATION_ITEM()
RATIONAL_B_SPLINE_CURVE((1.02428162962094,1.02311336089455,1.02147610369988))
REPRESENTATION_ITEM('')
);
#319=(
BOUNDED_CURVE()
B_SPLINE_CURVE(2,(#34603,#34604,#34605),.UNSPECIFIED.,.F.,.F.)
B_SPLINE_CURVE_WITH_KNOTS((3,3),(-0.271795897845348,-0.270098893534579),
 .UNSPECIFIED.)
CURVE()
GEOMETRIC_REPRESENTATION_ITEM()
RATIONAL_B_SPLINE_CURVE((1.02428162962101,1.02424425804592,1.02420640656119))
REPRESENTATION_ITEM('')
);
#320=(
BOUNDED_CURVE()
B_SPLINE_CURVE(2,(#34610,#34611,#34612),.UNSPECIFIED.,.F.,.F.)
B_SPLINE_CURVE_WITH_KNOTS((3,3),(-0.270098893534579,-0.218746031477162),
 .UNSPECIFIED.)
CURVE()
GEOMETRIC_REPRESENTATION_ITEM()
RATIONAL_B_SPLINE_CURVE((1.02420640656119,1.02306098691694,1.02147610369995))
REPRESENTATION_ITEM('')
);
#321=(
BOUNDED_CURVE()
B_SPLINE_CURVE(2,(#34614,#34615,#34616),.UNSPECIFIED.,.F.,.F.)
B_SPLINE_CURVE_WITH_KNOTS((3,3),(0.536094506482409,0.589144372850596),
 .UNSPECIFIED.)
CURVE()
GEOMETRIC_REPRESENTATION_ITEM()
RATIONAL_B_SPLINE_CURVE((1.02428162962102,1.02311336089463,1.02147610369996))
REPRESENTATION_ITEM('')
);
#322=(
BOUNDED_CURVE()
B_SPLINE_CURVE(2,(#34620,#34621,#34622),.UNSPECIFIED.,.F.,.F.)
B_SPLINE_CURVE_WITH_KNOTS((3,3),(0.21874603147716,0.271795897845345),
 .UNSPECIFIED.)
CURVE()
GEOMETRIC_REPRESENTATION_ITEM()
RATIONAL_B_SPLINE_CURVE((1.02147610369993,1.0231133608946,1.02428162962099))
REPRESENTATION_ITEM('')
);
#323=(
BOUNDED_CURVE()
B_SPLINE_CURVE(2,(#34624,#34625,#34626),.UNSPECIFIED.,.F.,.F.)
B_SPLINE_CURVE_WITH_KNOTS((3,3),(0.5360945064824,0.589144372850584),
 .UNSPECIFIED.)
CURVE()
GEOMETRIC_REPRESENTATION_ITEM()
RATIONAL_B_SPLINE_CURVE((1.02428162962094,1.02311336089455,1.02147610369988))
REPRESENTATION_ITEM('')
);
#324=(
BOUNDED_CURVE()
B_SPLINE_CURVE(2,(#34630,#34631,#34632),.UNSPECIFIED.,.F.,.F.)
B_SPLINE_CURVE_WITH_KNOTS((3,3),(0.218746031477174,0.271795897845361),
 .UNSPECIFIED.)
CURVE()
GEOMETRIC_REPRESENTATION_ITEM()
RATIONAL_B_SPLINE_CURVE((1.02147610369996,1.02311336089464,1.02428162962103))
REPRESENTATION_ITEM('')
);
#325=(
BOUNDED_CURVE()
B_SPLINE_CURVE(2,(#34634,#34635,#34636),.UNSPECIFIED.,.F.,.F.)
B_SPLINE_CURVE_WITH_KNOTS((3,3),(0.536094506482401,0.589144372850589),
 .UNSPECIFIED.)
CURVE()
GEOMETRIC_REPRESENTATION_ITEM()
RATIONAL_B_SPLINE_CURVE((1.02428162962104,1.02311336089465,1.02147610369997))
REPRESENTATION_ITEM('')
);
#326=(
BOUNDED_CURVE()
B_SPLINE_CURVE(2,(#34640,#34641,#34642),.UNSPECIFIED.,.F.,.F.)
B_SPLINE_CURVE_WITH_KNOTS((3,3),(0.218746031477168,0.271795897845352),
 .UNSPECIFIED.)
CURVE()
GEOMETRIC_REPRESENTATION_ITEM()
RATIONAL_B_SPLINE_CURVE((1.02147610369989,1.02311336089456,1.02428162962095))
REPRESENTATION_ITEM('')
);
#327=(
BOUNDED_CURVE()
B_SPLINE_CURVE(2,(#34644,#34645,#34646),.UNSPECIFIED.,.F.,.F.)
B_SPLINE_CURVE_WITH_KNOTS((3,3),(0.536094506482407,0.589144372850594),
 .UNSPECIFIED.)
CURVE()
GEOMETRIC_REPRESENTATION_ITEM()
RATIONAL_B_SPLINE_CURVE((1.02428162962103,1.02311336089464,1.02147610369996))
REPRESENTATION_ITEM('')
);
#328=(
BOUNDED_CURVE()
B_SPLINE_CURVE(2,(#34650,#34651,#34652),.UNSPECIFIED.,.F.,.F.)
B_SPLINE_CURVE_WITH_KNOTS((3,3),(0.218746031477174,0.27179589784536),
 .UNSPECIFIED.)
CURVE()
GEOMETRIC_REPRESENTATION_ITEM()
RATIONAL_B_SPLINE_CURVE((1.02147610369993,1.02311336089461,1.024281629621))
REPRESENTATION_ITEM('')
);
#329=(
BOUNDED_CURVE()
B_SPLINE_CURVE(2,(#34654,#34655,#34656),.UNSPECIFIED.,.F.,.F.)
B_SPLINE_CURVE_WITH_KNOTS((3,3),(0.536094506482403,0.589144372850591),
 .UNSPECIFIED.)
CURVE()
GEOMETRIC_REPRESENTATION_ITEM()
RATIONAL_B_SPLINE_CURVE((1.02428162962104,1.02311336089464,1.02147610369997))
REPRESENTATION_ITEM('')
);
#330=(
BOUNDED_CURVE()
B_SPLINE_CURVE(2,(#34660,#34661,#34662),.UNSPECIFIED.,.F.,.F.)
B_SPLINE_CURVE_WITH_KNOTS((3,3),(0.218746031477165,0.271795897845354),
 .UNSPECIFIED.)
CURVE()
GEOMETRIC_REPRESENTATION_ITEM()
RATIONAL_B_SPLINE_CURVE((1.02147610370001,1.02311336089469,1.02428162962109))
REPRESENTATION_ITEM('')
);
#331=(
BOUNDED_CURVE()
B_SPLINE_CURVE(2,(#34664,#34665,#34666),.UNSPECIFIED.,.F.,.F.)
B_SPLINE_CURVE_WITH_KNOTS((3,3),(0.536094506482406,0.589144372850589),
 .UNSPECIFIED.)
CURVE()
GEOMETRIC_REPRESENTATION_ITEM()
RATIONAL_B_SPLINE_CURVE((1.02428162962095,1.02311336089456,1.02147610369989))
REPRESENTATION_ITEM('')
);
#332=(
BOUNDED_CURVE()
B_SPLINE_CURVE(2,(#34670,#34671,#34672),.UNSPECIFIED.,.F.,.F.)
B_SPLINE_CURVE_WITH_KNOTS((3,3),(0.218746031477167,0.271795897845354),
 .UNSPECIFIED.)
CURVE()
GEOMETRIC_REPRESENTATION_ITEM()
RATIONAL_B_SPLINE_CURVE((1.02147610369995,1.02311336089462,1.02428162962101))
REPRESENTATION_ITEM('')
);
#333=(
BOUNDED_CURVE()
B_SPLINE_CURVE(2,(#34674,#34675,#34676),.UNSPECIFIED.,.F.,.F.)
B_SPLINE_CURVE_WITH_KNOTS((3,3),(0.536094506482406,0.58914437285059),
 .UNSPECIFIED.)
CURVE()
GEOMETRIC_REPRESENTATION_ITEM()
RATIONAL_B_SPLINE_CURVE((1.02428162962094,1.02311336089456,1.02147610369988))
REPRESENTATION_ITEM('')
);
#334=(
BOUNDED_CURVE()
B_SPLINE_CURVE(2,(#34680,#34681,#34682),.UNSPECIFIED.,.F.,.F.)
B_SPLINE_CURVE_WITH_KNOTS((3,3),(0.218746031477163,0.271795897845349),
 .UNSPECIFIED.)
CURVE()
GEOMETRIC_REPRESENTATION_ITEM()
RATIONAL_B_SPLINE_CURVE((1.02147610369995,1.02311336089462,1.02428162962102))
REPRESENTATION_ITEM('')
);
#335=(
BOUNDED_CURVE()
B_SPLINE_CURVE(2,(#34684,#34685,#34686),.UNSPECIFIED.,.F.,.F.)
B_SPLINE_CURVE_WITH_KNOTS((3,3),(0.536094506482405,0.58914437285059),
 .UNSPECIFIED.)
CURVE()
GEOMETRIC_REPRESENTATION_ITEM()
RATIONAL_B_SPLINE_CURVE((1.02428162962098,1.02311336089459,1.02147610369992))
REPRESENTATION_ITEM('')
);
#336=(
BOUNDED_CURVE()
B_SPLINE_CURVE(2,(#34690,#34691,#34692),.UNSPECIFIED.,.F.,.F.)
B_SPLINE_CURVE_WITH_KNOTS((3,3),(0.21874603147717,0.271795897845354),
 .UNSPECIFIED.)
CURVE()
GEOMETRIC_REPRESENTATION_ITEM()
RATIONAL_B_SPLINE_CURVE((1.0214761036999,1.02311336089457,1.02428162962096))
REPRESENTATION_ITEM('')
);
#337=(
BOUNDED_CURVE()
B_SPLINE_CURVE(2,(#34694,#34695,#34696),.UNSPECIFIED.,.F.,.F.)
B_SPLINE_CURVE_WITH_KNOTS((3,3),(0.536094506482405,0.589144372850589),
 .UNSPECIFIED.)
CURVE()
GEOMETRIC_REPRESENTATION_ITEM()
RATIONAL_B_SPLINE_CURVE((1.02428162962096,1.02311336089458,1.0214761036999))
REPRESENTATION_ITEM('')
);
#338=(
BOUNDED_CURVE()
B_SPLINE_CURVE(2,(#34700,#34701,#34702),.UNSPECIFIED.,.F.,.F.)
B_SPLINE_CURVE_WITH_KNOTS((3,3),(0.218746031477176,0.271795897845357),
 .UNSPECIFIED.)
CURVE()
GEOMETRIC_REPRESENTATION_ITEM()
RATIONAL_B_SPLINE_CURVE((1.02147610369985,1.02311336089452,1.02428162962091))
REPRESENTATION_ITEM('')
);
#339=(
BOUNDED_CURVE()
B_SPLINE_CURVE(2,(#34704,#34705,#34706),.UNSPECIFIED.,.F.,.F.)
B_SPLINE_CURVE_WITH_KNOTS((3,3),(0.536094506482407,0.589144372850591),
 .UNSPECIFIED.)
CURVE()
GEOMETRIC_REPRESENTATION_ITEM()
RATIONAL_B_SPLINE_CURVE((1.02428162962095,1.02311336089456,1.02147610369989))
REPRESENTATION_ITEM('')
);
#340=(
BOUNDED_CURVE()
B_SPLINE_CURVE(2,(#34710,#34711,#34712),.UNSPECIFIED.,.F.,.F.)
B_SPLINE_CURVE_WITH_KNOTS((3,3),(0.218746031477161,0.271795897845349),
 .UNSPECIFIED.)
CURVE()
GEOMETRIC_REPRESENTATION_ITEM()
RATIONAL_B_SPLINE_CURVE((1.02147610369998,1.02311336089466,1.02428162962106))
REPRESENTATION_ITEM('')
);
#341=(
BOUNDED_CURVE()
B_SPLINE_CURVE(2,(#34714,#34715,#34716),.UNSPECIFIED.,.F.,.F.)
B_SPLINE_CURVE_WITH_KNOTS((3,3),(0.536094506482414,0.589144372850592),
 .UNSPECIFIED.)
CURVE()
GEOMETRIC_REPRESENTATION_ITEM()
RATIONAL_B_SPLINE_CURVE((1.02428162962083,1.02311336089444,1.02147610369978))
REPRESENTATION_ITEM('')
);
#342=(
BOUNDED_CURVE()
B_SPLINE_CURVE(2,(#34720,#34721,#34722),.UNSPECIFIED.,.F.,.F.)
B_SPLINE_CURVE_WITH_KNOTS((3,3),(0.218746031477167,0.271795897845358),
 .UNSPECIFIED.)
CURVE()
GEOMETRIC_REPRESENTATION_ITEM()
RATIONAL_B_SPLINE_CURVE((1.02147610370001,1.02311336089469,1.02428162962108))
REPRESENTATION_ITEM('')
);
#343=(
BOUNDED_CURVE()
B_SPLINE_CURVE(2,(#34724,#34725,#34726),.UNSPECIFIED.,.F.,.F.)
B_SPLINE_CURVE_WITH_KNOTS((3,3),(0.536094506482411,0.589144372850593),
 .UNSPECIFIED.)
CURVE()
GEOMETRIC_REPRESENTATION_ITEM()
RATIONAL_B_SPLINE_CURVE((1.02428162962092,1.02311336089453,1.02147610369986))
REPRESENTATION_ITEM('')
);
#344=(
BOUNDED_CURVE()
B_SPLINE_CURVE(2,(#34730,#34731,#34732),.UNSPECIFIED.,.F.,.F.)
B_SPLINE_CURVE_WITH_KNOTS((3,3),(0.21874603147718,0.27179589784536),
 .UNSPECIFIED.)
CURVE()
GEOMETRIC_REPRESENTATION_ITEM()
RATIONAL_B_SPLINE_CURVE((1.02147610369982,1.02311336089449,1.02428162962087))
REPRESENTATION_ITEM('')
);
#345=(
BOUNDED_CURVE()
B_SPLINE_CURVE(2,(#34734,#34735,#34736),.UNSPECIFIED.,.F.,.F.)
B_SPLINE_CURVE_WITH_KNOTS((3,3),(0.536094506482394,0.589144372850576),
 .UNSPECIFIED.)
CURVE()
GEOMETRIC_REPRESENTATION_ITEM()
RATIONAL_B_SPLINE_CURVE((1.0242816296209,1.02311336089451,1.02147610369985))
REPRESENTATION_ITEM('')
);
#346=(
BOUNDED_CURVE()
B_SPLINE_CURVE(2,(#34740,#34741,#34742),.UNSPECIFIED.,.F.,.F.)
B_SPLINE_CURVE_WITH_KNOTS((3,3),(0.218746031477168,0.271795897845353),
 .UNSPECIFIED.)
CURVE()
GEOMETRIC_REPRESENTATION_ITEM()
RATIONAL_B_SPLINE_CURVE((1.02147610369992,1.0231133608946,1.02428162962099))
REPRESENTATION_ITEM('')
);
#347=(
BOUNDED_CURVE()
B_SPLINE_CURVE(2,(#34744,#34745,#34746),.UNSPECIFIED.,.F.,.F.)
B_SPLINE_CURVE_WITH_KNOTS((3,3),(0.536094506482401,0.589144372850586),
 .UNSPECIFIED.)
CURVE()
GEOMETRIC_REPRESENTATION_ITEM()
RATIONAL_B_SPLINE_CURVE((1.02428162962097,1.02311336089458,1.02147610369991))
REPRESENTATION_ITEM('')
);
#348=(
BOUNDED_CURVE()
B_SPLINE_CURVE(2,(#34750,#34751,#34752),.UNSPECIFIED.,.F.,.F.)
B_SPLINE_CURVE_WITH_KNOTS((3,3),(0.218746031477169,0.271795897845357),
 .UNSPECIFIED.)
CURVE()
GEOMETRIC_REPRESENTATION_ITEM()
RATIONAL_B_SPLINE_CURVE((1.02147610369996,1.02311336089463,1.02428162962103))
REPRESENTATION_ITEM('')
);
#349=(
BOUNDED_CURVE()
B_SPLINE_CURVE(2,(#34754,#34755,#34756),.UNSPECIFIED.,.F.,.F.)
B_SPLINE_CURVE_WITH_KNOTS((3,3),(0.53609450648239,0.589144372850573),
 .UNSPECIFIED.)
CURVE()
GEOMETRIC_REPRESENTATION_ITEM()
RATIONAL_B_SPLINE_CURVE((1.02428162962093,1.02311336089454,1.02147610369987))
REPRESENTATION_ITEM('')
);
#350=(
BOUNDED_CURVE()
B_SPLINE_CURVE(2,(#34760,#34761,#34762),.UNSPECIFIED.,.F.,.F.)
B_SPLINE_CURVE_WITH_KNOTS((3,3),(0.218746031477159,0.271795897845342),
 .UNSPECIFIED.)
CURVE()
GEOMETRIC_REPRESENTATION_ITEM()
RATIONAL_B_SPLINE_CURVE((1.02147610369989,1.02311336089456,1.02428162962095))
REPRESENTATION_ITEM('')
);
#351=(
BOUNDED_CURVE()
B_SPLINE_CURVE(2,(#34764,#34765,#34766),.UNSPECIFIED.,.F.,.F.)
B_SPLINE_CURVE_WITH_KNOTS((3,3),(0.536094506482392,0.58914437285058),
 .UNSPECIFIED.)
CURVE()
GEOMETRIC_REPRESENTATION_ITEM()
RATIONAL_B_SPLINE_CURVE((1.02428162962103,1.02311336089464,1.02147610369996))
REPRESENTATION_ITEM('')
);
#352=(
BOUNDED_CURVE()
B_SPLINE_CURVE(2,(#34770,#34771,#34772),.UNSPECIFIED.,.F.,.F.)
B_SPLINE_CURVE_WITH_KNOTS((3,3),(0.218746031477161,0.271795897845349),
 .UNSPECIFIED.)
CURVE()
GEOMETRIC_REPRESENTATION_ITEM()
RATIONAL_B_SPLINE_CURVE((1.02147610369998,1.02311336089466,1.02428162962105))
REPRESENTATION_ITEM('')
);
#353=(
BOUNDED_CURVE()
B_SPLINE_CURVE(2,(#34774,#34775,#34776),.UNSPECIFIED.,.F.,.F.)
B_SPLINE_CURVE_WITH_KNOTS((3,3),(0.536094506482406,0.589144372850593),
 .UNSPECIFIED.)
CURVE()
GEOMETRIC_REPRESENTATION_ITEM()
RATIONAL_B_SPLINE_CURVE((1.024281629621,1.02311336089461,1.02147610369993))
REPRESENTATION_ITEM('')
);
#354=(
BOUNDED_CURVE()
B_SPLINE_CURVE(2,(#34780,#34781,#34782),.UNSPECIFIED.,.F.,.F.)
B_SPLINE_CURVE_WITH_KNOTS((3,3),(0.218746031477174,0.271795897845361),
 .UNSPECIFIED.)
CURVE()
GEOMETRIC_REPRESENTATION_ITEM()
RATIONAL_B_SPLINE_CURVE((1.02147610369995,1.02311336089462,1.02428162962101))
REPRESENTATION_ITEM('')
);
#355=(
BOUNDED_CURVE()
B_SPLINE_CURVE(2,(#34784,#34785,#34786),.UNSPECIFIED.,.F.,.F.)
B_SPLINE_CURVE_WITH_KNOTS((3,3),(0.536094506482403,0.589144372850589),
 .UNSPECIFIED.)
CURVE()
GEOMETRIC_REPRESENTATION_ITEM()
RATIONAL_B_SPLINE_CURVE((1.02428162962099,1.0231133608946,1.02147610369993))
REPRESENTATION_ITEM('')
);
#356=(
BOUNDED_CURVE()
B_SPLINE_CURVE(2,(#34790,#34791,#34792),.UNSPECIFIED.,.F.,.F.)
B_SPLINE_CURVE_WITH_KNOTS((3,3),(0.218746031477177,0.271795897845364),
 .UNSPECIFIED.)
CURVE()
GEOMETRIC_REPRESENTATION_ITEM()
RATIONAL_B_SPLINE_CURVE((1.0214761036999,1.02311336089457,1.02428162962096))
REPRESENTATION_ITEM('')
);
#357=(
BOUNDED_CURVE()
B_SPLINE_CURVE(2,(#34794,#34795,#34796),.UNSPECIFIED.,.F.,.F.)
B_SPLINE_CURVE_WITH_KNOTS((3,3),(0.536094506482414,0.589144372850605),
 .UNSPECIFIED.)
CURVE()
GEOMETRIC_REPRESENTATION_ITEM()
RATIONAL_B_SPLINE_CURVE((1.02428162962111,1.02311336089472,1.02147610370003))
REPRESENTATION_ITEM('')
);
#358=(
BOUNDED_CURVE()
B_SPLINE_CURVE(2,(#34800,#34801,#34802),.UNSPECIFIED.,.F.,.F.)
B_SPLINE_CURVE_WITH_KNOTS((3,3),(0.218746031477174,0.271795897845363),
 .UNSPECIFIED.)
CURVE()
GEOMETRIC_REPRESENTATION_ITEM()
RATIONAL_B_SPLINE_CURVE((1.02147610369998,1.02311336089465,1.02428162962105))
REPRESENTATION_ITEM('')
);
#359=(
BOUNDED_CURVE()
B_SPLINE_CURVE(2,(#34804,#34805,#34806),.UNSPECIFIED.,.F.,.F.)
B_SPLINE_CURVE_WITH_KNOTS((3,3),(0.536094506482404,0.589144372850588),
 .UNSPECIFIED.)
CURVE()
GEOMETRIC_REPRESENTATION_ITEM()
RATIONAL_B_SPLINE_CURVE((1.02428162962096,1.02311336089458,1.0214761036999))
REPRESENTATION_ITEM('')
);
#360=(
BOUNDED_CURVE()
B_SPLINE_CURVE(2,(#34810,#34811,#34812),.UNSPECIFIED.,.F.,.F.)
B_SPLINE_CURVE_WITH_KNOTS((3,3),(0.218746031477183,0.271795897845364),
 .UNSPECIFIED.)
CURVE()
GEOMETRIC_REPRESENTATION_ITEM()
RATIONAL_B_SPLINE_CURVE((1.02147610369985,1.02311336089452,1.0242816296209))
REPRESENTATION_ITEM('')
);
#361=(
BOUNDED_CURVE()
B_SPLINE_CURVE(2,(#34814,#34815,#34816),.UNSPECIFIED.,.F.,.F.)
B_SPLINE_CURVE_WITH_KNOTS((3,3),(0.536094506482398,0.589144372850582),
 .UNSPECIFIED.)
CURVE()
GEOMETRIC_REPRESENTATION_ITEM()
RATIONAL_B_SPLINE_CURVE((1.02428162962094,1.02311336089455,1.02147610369988))
REPRESENTATION_ITEM('')
);
#362=(
BOUNDED_CURVE()
B_SPLINE_CURVE(2,(#34820,#34821,#34822),.UNSPECIFIED.,.F.,.F.)
B_SPLINE_CURVE_WITH_KNOTS((3,3),(0.21874603147717,0.271795897845347),
 .UNSPECIFIED.)
CURVE()
GEOMETRIC_REPRESENTATION_ITEM()
RATIONAL_B_SPLINE_CURVE((1.0214761036998,1.02311336089446,1.02428162962084))
REPRESENTATION_ITEM('')
);
#363=(
BOUNDED_CURVE()
B_SPLINE_CURVE(2,(#34824,#34825,#34826),.UNSPECIFIED.,.F.,.F.)
B_SPLINE_CURVE_WITH_KNOTS((3,3),(0.536094506482403,0.589144372850584),
 .UNSPECIFIED.)
CURVE()
GEOMETRIC_REPRESENTATION_ITEM()
RATIONAL_B_SPLINE_CURVE((1.02428162962089,1.02311336089451,1.02147610369984))
REPRESENTATION_ITEM('')
);
#364=(
BOUNDED_CURVE()
B_SPLINE_CURVE(2,(#34830,#34831,#34832),.UNSPECIFIED.,.F.,.F.)
B_SPLINE_CURVE_WITH_KNOTS((3,3),(0.218746031477161,0.271795897845346),
 .UNSPECIFIED.)
CURVE()
GEOMETRIC_REPRESENTATION_ITEM()
RATIONAL_B_SPLINE_CURVE((1.02147610369993,1.0231133608946,1.024281629621))
REPRESENTATION_ITEM('')
);
#365=(
BOUNDED_CURVE()
B_SPLINE_CURVE(2,(#34834,#34835,#34836),.UNSPECIFIED.,.F.,.F.)
B_SPLINE_CURVE_WITH_KNOTS((3,3),(0.53609450648241,0.589144372850597),
 .UNSPECIFIED.)
CURVE()
GEOMETRIC_REPRESENTATION_ITEM()
RATIONAL_B_SPLINE_CURVE((1.02428162962105,1.02311336089465,1.02147610369997))
REPRESENTATION_ITEM('')
);
#366=(
BOUNDED_CURVE()
B_SPLINE_CURVE(2,(#34840,#34841,#34842),.UNSPECIFIED.,.F.,.F.)
B_SPLINE_CURVE_WITH_KNOTS((3,3),(0.21874603147718,0.271795897845363),
 .UNSPECIFIED.)
CURVE()
GEOMETRIC_REPRESENTATION_ITEM()
RATIONAL_B_SPLINE_CURVE((1.02147610369987,1.02311336089453,1.02428162962092))
REPRESENTATION_ITEM('')
);
#367=(
BOUNDED_CURVE()
B_SPLINE_CURVE(2,(#34844,#34845,#34846),.UNSPECIFIED.,.F.,.F.)
B_SPLINE_CURVE_WITH_KNOTS((3,3),(0.536094506482391,0.589144372850573),
 .UNSPECIFIED.)
CURVE()
GEOMETRIC_REPRESENTATION_ITEM()
RATIONAL_B_SPLINE_CURVE((1.02428162962087,1.02311336089449,1.02147610369982))
REPRESENTATION_ITEM('')
);
#368=(
BOUNDED_CURVE()
B_SPLINE_CURVE(2,(#34850,#34851,#34852),.UNSPECIFIED.,.F.,.F.)
B_SPLINE_CURVE_WITH_KNOTS((3,3),(0.218746031477181,0.271795897845364),
 .UNSPECIFIED.)
CURVE()
GEOMETRIC_REPRESENTATION_ITEM()
RATIONAL_B_SPLINE_CURVE((1.02147610369986,1.02311336089452,1.02428162962091))
REPRESENTATION_ITEM('')
);
#369=(
BOUNDED_CURVE()
B_SPLINE_CURVE(2,(#34854,#34855,#34856),.UNSPECIFIED.,.F.,.F.)
B_SPLINE_CURVE_WITH_KNOTS((3,3),(0.536094506482413,0.589144372850602),
 .UNSPECIFIED.)
CURVE()
GEOMETRIC_REPRESENTATION_ITEM()
RATIONAL_B_SPLINE_CURVE((1.02428162962106,1.02311336089467,1.02147610369999))
REPRESENTATION_ITEM('')
);
#370=(
BOUNDED_CURVE()
B_SPLINE_CURVE(2,(#34860,#34861,#34862),.UNSPECIFIED.,.F.,.F.)
B_SPLINE_CURVE_WITH_KNOTS((3,3),(0.218746031477165,0.271795897845346),
 .UNSPECIFIED.)
CURVE()
GEOMETRIC_REPRESENTATION_ITEM()
RATIONAL_B_SPLINE_CURVE((1.02147610369987,1.02311336089454,1.02428162962093))
REPRESENTATION_ITEM('')
);
#371=(
BOUNDED_CURVE()
B_SPLINE_CURVE(2,(#34864,#34865,#34866),.UNSPECIFIED.,.F.,.F.)
B_SPLINE_CURVE_WITH_KNOTS((3,3),(0.53609450648241,0.589144372850598),
 .UNSPECIFIED.)
CURVE()
GEOMETRIC_REPRESENTATION_ITEM()
RATIONAL_B_SPLINE_CURVE((1.02428162962105,1.02311336089466,1.02147610369998))
REPRESENTATION_ITEM('')
);
#372=(
BOUNDED_CURVE()
B_SPLINE_CURVE(2,(#34870,#34871,#34872),.UNSPECIFIED.,.F.,.F.)
B_SPLINE_CURVE_WITH_KNOTS((3,3),(0.21874603147717,0.271795897845357),
 .UNSPECIFIED.)
CURVE()
GEOMETRIC_REPRESENTATION_ITEM()
RATIONAL_B_SPLINE_CURVE((1.02147610369995,1.02311336089463,1.02428162962102))
REPRESENTATION_ITEM('')
);
#373=(
BOUNDED_CURVE()
B_SPLINE_CURVE(2,(#34874,#34875,#34876),.UNSPECIFIED.,.F.,.F.)
B_SPLINE_CURVE_WITH_KNOTS((3,3),(0.536094506482409,0.589144372850597),
 .UNSPECIFIED.)
CURVE()
GEOMETRIC_REPRESENTATION_ITEM()
RATIONAL_B_SPLINE_CURVE((1.02428162962106,1.02311336089466,1.02147610369998))
REPRESENTATION_ITEM('')
);
#374=(
BOUNDED_CURVE()
B_SPLINE_CURVE(2,(#34880,#34881,#34882),.UNSPECIFIED.,.F.,.F.)
B_SPLINE_CURVE_WITH_KNOTS((3,3),(0.21874603147717,0.271795897845356),
 .UNSPECIFIED.)
CURVE()
GEOMETRIC_REPRESENTATION_ITEM()
RATIONAL_B_SPLINE_CURVE((1.02147610369992,1.02311336089459,1.02428162962098))
REPRESENTATION_ITEM('')
);
#375=(
BOUNDED_CURVE()
B_SPLINE_CURVE(2,(#34884,#34885,#34886),.UNSPECIFIED.,.F.,.F.)
B_SPLINE_CURVE_WITH_KNOTS((3,3),(0.536094506482409,0.589144372850597),
 .UNSPECIFIED.)
CURVE()
GEOMETRIC_REPRESENTATION_ITEM()
RATIONAL_B_SPLINE_CURVE((1.02428162962106,1.02311336089467,1.02147610369999))
REPRESENTATION_ITEM('')
);
#376=(
BOUNDED_CURVE()
B_SPLINE_CURVE(2,(#34890,#34891,#34892),.UNSPECIFIED.,.F.,.F.)
B_SPLINE_CURVE_WITH_KNOTS((3,3),(0.218746031477176,0.271795897845358),
 .UNSPECIFIED.)
CURVE()
GEOMETRIC_REPRESENTATION_ITEM()
RATIONAL_B_SPLINE_CURVE((1.02147610369985,1.02311336089452,1.0242816296209))
REPRESENTATION_ITEM('')
);
#377=(
BOUNDED_CURVE()
B_SPLINE_CURVE(2,(#34894,#34895,#34896),.UNSPECIFIED.,.F.,.F.)
B_SPLINE_CURVE_WITH_KNOTS((3,3),(0.536094506482385,0.589144372850568),
 .UNSPECIFIED.)
CURVE()
GEOMETRIC_REPRESENTATION_ITEM()
RATIONAL_B_SPLINE_CURVE((1.02428162962089,1.0231133608945,1.02147610369984))
REPRESENTATION_ITEM('')
);
#378=(
BOUNDED_CURVE()
B_SPLINE_CURVE(2,(#34900,#34901,#34902),.UNSPECIFIED.,.F.,.F.)
B_SPLINE_CURVE_WITH_KNOTS((3,3),(0.218746031477173,0.271795897845358),
 .UNSPECIFIED.)
CURVE()
GEOMETRIC_REPRESENTATION_ITEM()
RATIONAL_B_SPLINE_CURVE((1.02147610369988,1.02311336089455,1.02428162962094))
REPRESENTATION_ITEM('')
);
#379=(
BOUNDED_CURVE()
B_SPLINE_CURVE(2,(#34904,#34905,#34906),.UNSPECIFIED.,.F.,.F.)
B_SPLINE_CURVE_WITH_KNOTS((3,3),(0.536094506482398,0.589144372850582),
 .UNSPECIFIED.)
CURVE()
GEOMETRIC_REPRESENTATION_ITEM()
RATIONAL_B_SPLINE_CURVE((1.02428162962091,1.02311336089453,1.02147610369986))
REPRESENTATION_ITEM('')
);
#380=(
BOUNDED_CURVE()
B_SPLINE_CURVE(2,(#34910,#34911,#34912),.UNSPECIFIED.,.F.,.F.)
B_SPLINE_CURVE_WITH_KNOTS((3,3),(0.218746031477167,0.271795897845352),
 .UNSPECIFIED.)
CURVE()
GEOMETRIC_REPRESENTATION_ITEM()
RATIONAL_B_SPLINE_CURVE((1.02147610369992,1.0231133608946,1.02428162962099))
REPRESENTATION_ITEM('')
);
#381=(
BOUNDED_CURVE()
B_SPLINE_CURVE(2,(#34914,#34915,#34916),.UNSPECIFIED.,.F.,.F.)
B_SPLINE_CURVE_WITH_KNOTS((3,3),(0.536094506482388,0.589144372850568),
 .UNSPECIFIED.)
CURVE()
GEOMETRIC_REPRESENTATION_ITEM()
RATIONAL_B_SPLINE_CURVE((1.02428162962083,1.02311336089444,1.02147610369978))
REPRESENTATION_ITEM('')
);
#382=(
BOUNDED_CURVE()
B_SPLINE_CURVE(2,(#34920,#34921,#34922),.UNSPECIFIED.,.F.,.F.)
B_SPLINE_CURVE_WITH_KNOTS((3,3),(0.218746031477159,0.271795897845343),
 .UNSPECIFIED.)
CURVE()
GEOMETRIC_REPRESENTATION_ITEM()
RATIONAL_B_SPLINE_CURVE((1.02147610369992,1.02311336089459,1.02428162962098))
REPRESENTATION_ITEM('')
);
#383=(
BOUNDED_CURVE()
B_SPLINE_CURVE(2,(#34924,#34925,#34926),.UNSPECIFIED.,.F.,.F.)
B_SPLINE_CURVE_WITH_KNOTS((3,3),(0.536094506482409,0.589144372850598),
 .UNSPECIFIED.)
CURVE()
GEOMETRIC_REPRESENTATION_ITEM()
RATIONAL_B_SPLINE_CURVE((1.02428162962104,1.02311336089465,1.02147610369997))
REPRESENTATION_ITEM('')
);
#384=(
BOUNDED_CURVE()
B_SPLINE_CURVE(2,(#34930,#34931,#34932),.UNSPECIFIED.,.F.,.F.)
B_SPLINE_CURVE_WITH_KNOTS((3,3),(0.218746031477167,0.271795897845353),
 .UNSPECIFIED.)
CURVE()
GEOMETRIC_REPRESENTATION_ITEM()
RATIONAL_B_SPLINE_CURVE((1.02147610369994,1.02311336089461,1.024281629621))
REPRESENTATION_ITEM('')
);
#385=(
BOUNDED_CURVE()
B_SPLINE_CURVE(2,(#34934,#34935,#34936),.UNSPECIFIED.,.F.,.F.)
B_SPLINE_CURVE_WITH_KNOTS((3,3),(0.536094506482415,0.589144372850595),
 .UNSPECIFIED.)
CURVE()
GEOMETRIC_REPRESENTATION_ITEM()
RATIONAL_B_SPLINE_CURVE((1.0242816296209,1.02311336089451,1.02147610369984))
REPRESENTATION_ITEM('')
);
#386=(
BOUNDED_CURVE()
B_SPLINE_CURVE(2,(#34940,#34941,#34942),.UNSPECIFIED.,.F.,.F.)
B_SPLINE_CURVE_WITH_KNOTS((3,3),(0.218746031477164,0.271795897845348),
 .UNSPECIFIED.)
CURVE()
GEOMETRIC_REPRESENTATION_ITEM()
RATIONAL_B_SPLINE_CURVE((1.02147610369991,1.02311336089458,1.02428162962097))
REPRESENTATION_ITEM('')
);
#387=(
BOUNDED_CURVE()
B_SPLINE_CURVE(2,(#34944,#34945,#34946),.UNSPECIFIED.,.F.,.F.)
B_SPLINE_CURVE_WITH_KNOTS((3,3),(0.536094506482408,0.589144372850597),
 .UNSPECIFIED.)
CURVE()
GEOMETRIC_REPRESENTATION_ITEM()
RATIONAL_B_SPLINE_CURVE((1.02428162962106,1.02311336089466,1.02147610369999))
REPRESENTATION_ITEM('')
);
#388=(
BOUNDED_CURVE()
B_SPLINE_CURVE(2,(#34950,#34951,#34952),.UNSPECIFIED.,.F.,.F.)
B_SPLINE_CURVE_WITH_KNOTS((3,3),(0.218746031477166,0.271795897845352),
 .UNSPECIFIED.)
CURVE()
GEOMETRIC_REPRESENTATION_ITEM()
RATIONAL_B_SPLINE_CURVE((1.02147610369992,1.0231133608946,1.02428162962099))
REPRESENTATION_ITEM('')
);
#389=(
BOUNDED_CURVE()
B_SPLINE_CURVE(2,(#34954,#34955,#34956),.UNSPECIFIED.,.F.,.F.)
B_SPLINE_CURVE_WITH_KNOTS((3,3),(0.536094506482395,0.589144372850571),
 .UNSPECIFIED.)
CURVE()
GEOMETRIC_REPRESENTATION_ITEM()
RATIONAL_B_SPLINE_CURVE((1.02428162962077,1.02311336089439,1.02147610369973))
REPRESENTATION_ITEM('')
);
#390=(
BOUNDED_CURVE()
B_SPLINE_CURVE(2,(#34960,#34961,#34962),.UNSPECIFIED.,.F.,.F.)
B_SPLINE_CURVE_WITH_KNOTS((3,3),(0.218746031477178,0.27179589784536),
 .UNSPECIFIED.)
CURVE()
GEOMETRIC_REPRESENTATION_ITEM()
RATIONAL_B_SPLINE_CURVE((1.02147610369982,1.02311336089448,1.02428162962087))
REPRESENTATION_ITEM('')
);
#391=(
BOUNDED_CURVE()
B_SPLINE_CURVE(2,(#34964,#34965,#34966),.UNSPECIFIED.,.F.,.F.)
B_SPLINE_CURVE_WITH_KNOTS((3,3),(0.536094506482417,0.589144372850603),
 .UNSPECIFIED.)
CURVE()
GEOMETRIC_REPRESENTATION_ITEM()
RATIONAL_B_SPLINE_CURVE((1.02428162962101,1.02311336089462,1.02147610369994))
REPRESENTATION_ITEM('')
);
#392=(
BOUNDED_CURVE()
B_SPLINE_CURVE(2,(#34970,#34971,#34972),.UNSPECIFIED.,.F.,.F.)
B_SPLINE_CURVE_WITH_KNOTS((3,3),(0.218746031477165,0.271795897845348),
 .UNSPECIFIED.)
CURVE()
GEOMETRIC_REPRESENTATION_ITEM()
RATIONAL_B_SPLINE_CURVE((1.02147610369987,1.02311336089454,1.02428162962093))
REPRESENTATION_ITEM('')
);
#393=(
BOUNDED_CURVE()
B_SPLINE_CURVE(2,(#34974,#34975,#34976),.UNSPECIFIED.,.F.,.F.)
B_SPLINE_CURVE_WITH_KNOTS((3,3),(0.536094506482408,0.589144372850592),
 .UNSPECIFIED.)
CURVE()
GEOMETRIC_REPRESENTATION_ITEM()
RATIONAL_B_SPLINE_CURVE((1.02428162962092,1.02311336089454,1.02147610369987))
REPRESENTATION_ITEM('')
);
#394=(
BOUNDED_CURVE()
B_SPLINE_CURVE(2,(#34980,#34981,#34982),.UNSPECIFIED.,.F.,.F.)
B_SPLINE_CURVE_WITH_KNOTS((3,3),(0.218746031477181,0.271795897845365),
 .UNSPECIFIED.)
CURVE()
GEOMETRIC_REPRESENTATION_ITEM()
RATIONAL_B_SPLINE_CURVE((1.02147610369986,1.02311336089453,1.02428162962092))
REPRESENTATION_ITEM('')
);
#395=(
BOUNDED_CURVE()
B_SPLINE_CURVE(2,(#34984,#34985,#34986),.UNSPECIFIED.,.F.,.F.)
B_SPLINE_CURVE_WITH_KNOTS((3,3),(0.536094506482407,0.589144372850588),
 .UNSPECIFIED.)
CURVE()
GEOMETRIC_REPRESENTATION_ITEM()
RATIONAL_B_SPLINE_CURVE((1.02428162962089,1.0231133608945,1.02147610369984))
REPRESENTATION_ITEM('')
);
#396=(
BOUNDED_CURVE()
B_SPLINE_CURVE(2,(#34989,#34990,#34991),.UNSPECIFIED.,.F.,.F.)
B_SPLINE_CURVE_WITH_KNOTS((3,3),(0.218746031477154,0.27179589784534),
 .UNSPECIFIED.)
CURVE()
GEOMETRIC_REPRESENTATION_ITEM()
RATIONAL_B_SPLINE_CURVE((1.02147610369997,1.02311336089464,1.02428162962104))
REPRESENTATION_ITEM('')
);
#397=(
BOUNDED_CURVE()
B_SPLINE_CURVE(2,(#34995,#34996,#34997),.UNSPECIFIED.,.F.,.F.)
B_SPLINE_CURVE_WITH_KNOTS((3,3),(0.536094506482396,0.589144372850575),
 .UNSPECIFIED.)
CURVE()
GEOMETRIC_REPRESENTATION_ITEM()
RATIONAL_B_SPLINE_CURVE((1.02428162962084,1.02311336089446,1.0214761036998))
REPRESENTATION_ITEM('')
);
#398=(
BOUNDED_CURVE()
B_SPLINE_CURVE(2,(#35001,#35002,#35003),.UNSPECIFIED.,.F.,.F.)
B_SPLINE_CURVE_WITH_KNOTS((3,3),(-0.271795897845359,-0.218746031477171),
 .UNSPECIFIED.)
CURVE()
GEOMETRIC_REPRESENTATION_ITEM()
RATIONAL_B_SPLINE_CURVE((1.02428162962104,1.02311336089465,1.02147610369997))
REPRESENTATION_ITEM('')
);
#399=(
BOUNDED_CURVE()
B_SPLINE_CURVE(2,(#35005,#35006,#35007),.UNSPECIFIED.,.F.,.F.)
B_SPLINE_CURVE_WITH_KNOTS((3,3),(-0.589144372850596,-0.536094506482412),
 .UNSPECIFIED.)
CURVE()
GEOMETRIC_REPRESENTATION_ITEM()
RATIONAL_B_SPLINE_CURVE((1.02147610369993,1.02311336089461,1.024281629621))
REPRESENTATION_ITEM('')
);
#400=(
BOUNDED_CURVE()
B_SPLINE_CURVE(2,(#35011,#35012,#35013),.UNSPECIFIED.,.F.,.F.)
B_SPLINE_CURVE_WITH_KNOTS((3,3),(-0.271795897845366,-0.218746031477182),
 .UNSPECIFIED.)
CURVE()
GEOMETRIC_REPRESENTATION_ITEM()
RATIONAL_B_SPLINE_CURVE((1.02428162962093,1.02311336089455,1.02147610369988))
REPRESENTATION_ITEM('')
);
#401=(
BOUNDED_CURVE()
B_SPLINE_CURVE(2,(#35015,#35016,#35017),.UNSPECIFIED.,.F.,.F.)
B_SPLINE_CURVE_WITH_KNOTS((3,3),(-0.589144372850618,-0.53609450648243),
 .UNSPECIFIED.)
CURVE()
GEOMETRIC_REPRESENTATION_ITEM()
RATIONAL_B_SPLINE_CURVE((1.02147610370001,1.02311336089469,1.02428162962108))
REPRESENTATION_ITEM('')
);
#402=(
BOUNDED_CURVE()
B_SPLINE_CURVE(2,(#35021,#35022,#35023),.UNSPECIFIED.,.F.,.F.)
B_SPLINE_CURVE_WITH_KNOTS((3,3),(-0.271795897845358,-0.218746031477173),
 .UNSPECIFIED.)
CURVE()
GEOMETRIC_REPRESENTATION_ITEM()
RATIONAL_B_SPLINE_CURVE((1.02428162962097,1.02311336089459,1.02147610369991))
REPRESENTATION_ITEM('')
);
#403=(
BOUNDED_CURVE()
B_SPLINE_CURVE(2,(#35025,#35026,#35027),.UNSPECIFIED.,.F.,.F.)
B_SPLINE_CURVE_WITH_KNOTS((3,3),(-0.589144372850595,-0.53609450648241),
 .UNSPECIFIED.)
CURVE()
GEOMETRIC_REPRESENTATION_ITEM()
RATIONAL_B_SPLINE_CURVE((1.02147610369992,1.0231133608946,1.02428162962099))
REPRESENTATION_ITEM('')
);
#404=(
BOUNDED_CURVE()
B_SPLINE_CURVE(2,(#35031,#35032,#35033),.UNSPECIFIED.,.F.,.F.)
B_SPLINE_CURVE_WITH_KNOTS((3,3),(-0.271795897845356,-0.218746031477171),
 .UNSPECIFIED.)
CURVE()
GEOMETRIC_REPRESENTATION_ITEM()
RATIONAL_B_SPLINE_CURVE((1.024281629621,1.02311336089461,1.02147610369993))
REPRESENTATION_ITEM('')
);
#405=(
BOUNDED_CURVE()
B_SPLINE_CURVE(2,(#35035,#35036,#35037),.UNSPECIFIED.,.F.,.F.)
B_SPLINE_CURVE_WITH_KNOTS((3,3),(-0.589144372850588,-0.536094506482404),
 .UNSPECIFIED.)
CURVE()
GEOMETRIC_REPRESENTATION_ITEM()
RATIONAL_B_SPLINE_CURVE((1.0214761036999,1.02311336089458,1.02428162962097))
REPRESENTATION_ITEM('')
);
#406=(
BOUNDED_CURVE()
B_SPLINE_CURVE(2,(#35041,#35042,#35043),.UNSPECIFIED.,.F.,.F.)
B_SPLINE_CURVE_WITH_KNOTS((3,3),(-0.271795897845343,-0.218746031477154),
 .UNSPECIFIED.)
CURVE()
GEOMETRIC_REPRESENTATION_ITEM()
RATIONAL_B_SPLINE_CURVE((1.02428162962107,1.02311336089467,1.02147610369999))
REPRESENTATION_ITEM('')
);
#407=(
BOUNDED_CURVE()
B_SPLINE_CURVE(2,(#35045,#35046,#35047),.UNSPECIFIED.,.F.,.F.)
B_SPLINE_CURVE_WITH_KNOTS((3,3),(-0.589144372850603,-0.536094506482417),
 .UNSPECIFIED.)
CURVE()
GEOMETRIC_REPRESENTATION_ITEM()
RATIONAL_B_SPLINE_CURVE((1.02147610369995,1.02311336089463,1.02428162962102))
REPRESENTATION_ITEM('')
);
#408=(
BOUNDED_CURVE()
B_SPLINE_CURVE(2,(#35051,#35052,#35053),.UNSPECIFIED.,.F.,.F.)
B_SPLINE_CURVE_WITH_KNOTS((3,3),(-0.271795897845354,-0.218746031477172),
 .UNSPECIFIED.)
CURVE()
GEOMETRIC_REPRESENTATION_ITEM()
RATIONAL_B_SPLINE_CURVE((1.02428162962093,1.02311336089455,1.02147610369988))
REPRESENTATION_ITEM('')
);
#409=(
BOUNDED_CURVE()
B_SPLINE_CURVE(2,(#35055,#35056,#35057),.UNSPECIFIED.,.F.,.F.)
B_SPLINE_CURVE_WITH_KNOTS((3,3),(-0.589144372850597,-0.536094506482412),
 .UNSPECIFIED.)
CURVE()
GEOMETRIC_REPRESENTATION_ITEM()
RATIONAL_B_SPLINE_CURVE((1.02147610369993,1.02311336089461,1.024281629621))
REPRESENTATION_ITEM('')
);
#410=(
BOUNDED_CURVE()
B_SPLINE_CURVE(2,(#35061,#35062,#35063),.UNSPECIFIED.,.F.,.F.)
B_SPLINE_CURVE_WITH_KNOTS((3,3),(-0.271795897845357,-0.218746031477169),
 .UNSPECIFIED.)
CURVE()
GEOMETRIC_REPRESENTATION_ITEM()
RATIONAL_B_SPLINE_CURVE((1.02428162962103,1.02311336089464,1.02147610369996))
REPRESENTATION_ITEM('')
);
#411=(
BOUNDED_CURVE()
B_SPLINE_CURVE(2,(#35065,#35066,#35067),.UNSPECIFIED.,.F.,.F.)
B_SPLINE_CURVE_WITH_KNOTS((3,3),(-0.589144372850578,-0.536094506482397),
 .UNSPECIFIED.)
CURVE()
GEOMETRIC_REPRESENTATION_ITEM()
RATIONAL_B_SPLINE_CURVE((1.02147610369984,1.02311336089451,1.02428162962089))
REPRESENTATION_ITEM('')
);
#412=(
BOUNDED_CURVE()
B_SPLINE_CURVE(2,(#35071,#35072,#35073),.UNSPECIFIED.,.F.,.F.)
B_SPLINE_CURVE_WITH_KNOTS((3,3),(-0.271795897845352,-0.21874603147717),
 .UNSPECIFIED.)
CURVE()
GEOMETRIC_REPRESENTATION_ITEM()
RATIONAL_B_SPLINE_CURVE((1.02428162962095,1.02311336089456,1.02147610369989))
REPRESENTATION_ITEM('')
);
#413=(
BOUNDED_CURVE()
B_SPLINE_CURVE(2,(#35075,#35076,#35077),.UNSPECIFIED.,.F.,.F.)
B_SPLINE_CURVE_WITH_KNOTS((3,3),(-0.589144372850593,-0.536094506482411),
 .UNSPECIFIED.)
CURVE()
GEOMETRIC_REPRESENTATION_ITEM()
RATIONAL_B_SPLINE_CURVE((1.02147610369986,1.02311336089453,1.02428162962091))
REPRESENTATION_ITEM('')
);
#414=(
BOUNDED_CURVE()
B_SPLINE_CURVE(2,(#35081,#35082,#35083),.UNSPECIFIED.,.F.,.F.)
B_SPLINE_CURVE_WITH_KNOTS((3,3),(-0.271795897845351,-0.218746031477166),
 .UNSPECIFIED.)
CURVE()
GEOMETRIC_REPRESENTATION_ITEM()
RATIONAL_B_SPLINE_CURVE((1.02428162962098,1.02311336089459,1.02147610369992))
REPRESENTATION_ITEM('')
);
#415=(
BOUNDED_CURVE()
B_SPLINE_CURVE(2,(#35085,#35086,#35087),.UNSPECIFIED.,.F.,.F.)
B_SPLINE_CURVE_WITH_KNOTS((3,3),(-0.589144372850585,-0.536094506482403),
 .UNSPECIFIED.)
CURVE()
GEOMETRIC_REPRESENTATION_ITEM()
RATIONAL_B_SPLINE_CURVE((1.02147610369985,1.02311336089452,1.02428162962091))
REPRESENTATION_ITEM('')
);
#416=(
BOUNDED_CURVE()
B_SPLINE_CURVE(2,(#35091,#35092,#35093),.UNSPECIFIED.,.F.,.F.)
B_SPLINE_CURVE_WITH_KNOTS((3,3),(-0.271795897845359,-0.218746031477178),
 .UNSPECIFIED.)
CURVE()
GEOMETRIC_REPRESENTATION_ITEM()
RATIONAL_B_SPLINE_CURVE((1.02428162962089,1.02311336089451,1.02147610369984))
REPRESENTATION_ITEM('')
);
#417=(
BOUNDED_CURVE()
B_SPLINE_CURVE(2,(#35095,#35096,#35097),.UNSPECIFIED.,.F.,.F.)
B_SPLINE_CURVE_WITH_KNOTS((3,3),(-0.589144372850604,-0.536094506482418),
 .UNSPECIFIED.)
CURVE()
GEOMETRIC_REPRESENTATION_ITEM()
RATIONAL_B_SPLINE_CURVE((1.02147610369994,1.02311336089462,1.02428162962101))
REPRESENTATION_ITEM('')
);
#418=(
BOUNDED_CURVE()
B_SPLINE_CURVE(2,(#35101,#35102,#35103),.UNSPECIFIED.,.F.,.F.)
B_SPLINE_CURVE_WITH_KNOTS((3,3),(-0.271795897845358,-0.218746031477175),
 .UNSPECIFIED.)
CURVE()
GEOMETRIC_REPRESENTATION_ITEM()
RATIONAL_B_SPLINE_CURVE((1.02428162962093,1.02311336089454,1.02147610369987))
REPRESENTATION_ITEM('')
);
#419=(
BOUNDED_CURVE()
B_SPLINE_CURVE(2,(#35105,#35106,#35107),.UNSPECIFIED.,.F.,.F.)
B_SPLINE_CURVE_WITH_KNOTS((3,3),(-0.589144372850589,-0.536094506482406),
 .UNSPECIFIED.)
CURVE()
GEOMETRIC_REPRESENTATION_ITEM()
RATIONAL_B_SPLINE_CURVE((1.02147610369989,1.02311336089456,1.02428162962095))
REPRESENTATION_ITEM('')
);
#420=(
BOUNDED_CURVE()
B_SPLINE_CURVE(2,(#35111,#35112,#35113),.UNSPECIFIED.,.F.,.F.)
B_SPLINE_CURVE_WITH_KNOTS((3,3),(-0.271795897845353,-0.218746031477168),
 .UNSPECIFIED.)
CURVE()
GEOMETRIC_REPRESENTATION_ITEM()
RATIONAL_B_SPLINE_CURVE((1.02428162962098,1.0231133608946,1.02147610369992))
REPRESENTATION_ITEM('')
);
#421=(
BOUNDED_CURVE()
B_SPLINE_CURVE(2,(#35115,#35116,#35117),.UNSPECIFIED.,.F.,.F.)
B_SPLINE_CURVE_WITH_KNOTS((3,3),(-0.589144372850587,-0.536094506482403),
 .UNSPECIFIED.)
CURVE()
GEOMETRIC_REPRESENTATION_ITEM()
RATIONAL_B_SPLINE_CURVE((1.02147610369986,1.02311336089453,1.02428162962092))
REPRESENTATION_ITEM('')
);
#422=(
BOUNDED_CURVE()
B_SPLINE_CURVE(2,(#35121,#35122,#35123),.UNSPECIFIED.,.F.,.F.)
B_SPLINE_CURVE_WITH_KNOTS((3,3),(-0.271795897845348,-0.218746031477167),
 .UNSPECIFIED.)
CURVE()
GEOMETRIC_REPRESENTATION_ITEM()
RATIONAL_B_SPLINE_CURVE((1.02428162962092,1.02311336089453,1.02147610369986))
REPRESENTATION_ITEM('')
);
#423=(
BOUNDED_CURVE()
B_SPLINE_CURVE(2,(#35125,#35126,#35127),.UNSPECIFIED.,.F.,.F.)
B_SPLINE_CURVE_WITH_KNOTS((3,3),(-0.589144372850583,-0.536094506482401),
 .UNSPECIFIED.)
CURVE()
GEOMETRIC_REPRESENTATION_ITEM()
RATIONAL_B_SPLINE_CURVE((1.02147610369985,1.02311336089452,1.0242816296209))
REPRESENTATION_ITEM('')
);
#424=(
BOUNDED_CURVE()
B_SPLINE_CURVE(2,(#35131,#35132,#35133),.UNSPECIFIED.,.F.,.F.)
B_SPLINE_CURVE_WITH_KNOTS((3,3),(-0.271795897845352,-0.218746031477164),
 .UNSPECIFIED.)
CURVE()
GEOMETRIC_REPRESENTATION_ITEM()
RATIONAL_B_SPLINE_CURVE((1.02428162962106,1.02311336089466,1.02147610369999))
REPRESENTATION_ITEM('')
);
#425=(
BOUNDED_CURVE()
B_SPLINE_CURVE(2,(#35135,#35136,#35137),.UNSPECIFIED.,.F.,.F.)
B_SPLINE_CURVE_WITH_KNOTS((3,3),(-0.589144372850585,-0.536094506482407),
 .UNSPECIFIED.)
CURVE()
GEOMETRIC_REPRESENTATION_ITEM()
RATIONAL_B_SPLINE_CURVE((1.02147610369979,1.02311336089446,1.02428162962084))
REPRESENTATION_ITEM('')
);
#426=(
BOUNDED_CURVE()
B_SPLINE_CURVE(2,(#35141,#35142,#35143),.UNSPECIFIED.,.F.,.F.)
B_SPLINE_CURVE_WITH_KNOTS((3,3),(-0.271795897845344,-0.21874603147716),
 .UNSPECIFIED.)
CURVE()
GEOMETRIC_REPRESENTATION_ITEM()
RATIONAL_B_SPLINE_CURVE((1.02428162962098,1.02311336089459,1.02147610369992))
REPRESENTATION_ITEM('')
);
#427=(
BOUNDED_CURVE()
B_SPLINE_CURVE(2,(#35145,#35146,#35147),.UNSPECIFIED.,.F.,.F.)
B_SPLINE_CURVE_WITH_KNOTS((3,3),(-0.589144372850594,-0.536094506482412),
 .UNSPECIFIED.)
CURVE()
GEOMETRIC_REPRESENTATION_ITEM()
RATIONAL_B_SPLINE_CURVE((1.02147610369985,1.02311336089452,1.02428162962091))
REPRESENTATION_ITEM('')
);
#428=(
BOUNDED_CURVE()
B_SPLINE_CURVE(2,(#35151,#35152,#35153),.UNSPECIFIED.,.F.,.F.)
B_SPLINE_CURVE_WITH_KNOTS((3,3),(-0.271795897845361,-0.218746031477178),
 .UNSPECIFIED.)
CURVE()
GEOMETRIC_REPRESENTATION_ITEM()
RATIONAL_B_SPLINE_CURVE((1.02428162962094,1.02311336089455,1.02147610369988))
REPRESENTATION_ITEM('')
);
#429=(
BOUNDED_CURVE()
B_SPLINE_CURVE(2,(#35155,#35156,#35157),.UNSPECIFIED.,.F.,.F.)
B_SPLINE_CURVE_WITH_KNOTS((3,3),(-0.589144372850589,-0.536094506482408),
 .UNSPECIFIED.)
CURVE()
GEOMETRIC_REPRESENTATION_ITEM()
RATIONAL_B_SPLINE_CURVE((1.02147610369984,1.02311336089451,1.02428162962089))
REPRESENTATION_ITEM('')
);
#430=(
BOUNDED_CURVE()
B_SPLINE_CURVE(2,(#35161,#35162,#35163),.UNSPECIFIED.,.F.,.F.)
B_SPLINE_CURVE_WITH_KNOTS((3,3),(-0.271795897845358,-0.218746031477168),
 .UNSPECIFIED.)
CURVE()
GEOMETRIC_REPRESENTATION_ITEM()
RATIONAL_B_SPLINE_CURVE((1.0242816296211,1.02311336089471,1.02147610370002))
REPRESENTATION_ITEM('')
);
#431=(
BOUNDED_CURVE()
B_SPLINE_CURVE(2,(#35165,#35166,#35167),.UNSPECIFIED.,.F.,.F.)
B_SPLINE_CURVE_WITH_KNOTS((3,3),(-0.5891443728506,-0.536094506482411),
 .UNSPECIFIED.)
CURVE()
GEOMETRIC_REPRESENTATION_ITEM()
RATIONAL_B_SPLINE_CURVE((1.02147610369999,1.02311336089467,1.02428162962106))
REPRESENTATION_ITEM('')
);
#432=(
BOUNDED_CURVE()
B_SPLINE_CURVE(2,(#35171,#35172,#35173),.UNSPECIFIED.,.F.,.F.)
B_SPLINE_CURVE_WITH_KNOTS((3,3),(-0.271795897845357,-0.218746031477171),
 .UNSPECIFIED.)
CURVE()
GEOMETRIC_REPRESENTATION_ITEM()
RATIONAL_B_SPLINE_CURVE((1.02428162962099,1.0231133608946,1.02147610369993))
REPRESENTATION_ITEM('')
);
#433=(
BOUNDED_CURVE()
B_SPLINE_CURVE(2,(#35175,#35176,#35177),.UNSPECIFIED.,.F.,.F.)
B_SPLINE_CURVE_WITH_KNOTS((3,3),(-0.589144372850592,-0.536094506482407),
 .UNSPECIFIED.)
CURVE()
GEOMETRIC_REPRESENTATION_ITEM()
RATIONAL_B_SPLINE_CURVE((1.02147610369992,1.0231133608946,1.02428162962099))
REPRESENTATION_ITEM('')
);
#434=(
BOUNDED_CURVE()
B_SPLINE_CURVE(2,(#35181,#35182,#35183),.UNSPECIFIED.,.F.,.F.)
B_SPLINE_CURVE_WITH_KNOTS((3,3),(-0.27179589784535,-0.218746031477161),
 .UNSPECIFIED.)
CURVE()
GEOMETRIC_REPRESENTATION_ITEM()
RATIONAL_B_SPLINE_CURVE((1.02428162962108,1.02311336089469,1.02147610370001))
REPRESENTATION_ITEM('')
);
#435=(
BOUNDED_CURVE()
B_SPLINE_CURVE(2,(#35185,#35186,#35187),.UNSPECIFIED.,.F.,.F.)
B_SPLINE_CURVE_WITH_KNOTS((3,3),(-0.589144372850596,-0.536094506482411),
 .UNSPECIFIED.)
CURVE()
GEOMETRIC_REPRESENTATION_ITEM()
RATIONAL_B_SPLINE_CURVE((1.02147610369991,1.02311336089458,1.02428162962097))
REPRESENTATION_ITEM('')
);
#436=(
BOUNDED_CURVE()
B_SPLINE_CURVE(2,(#35191,#35192,#35193),.UNSPECIFIED.,.F.,.F.)
B_SPLINE_CURVE_WITH_KNOTS((3,3),(-0.271795897845359,-0.218746031477175),
 .UNSPECIFIED.)
CURVE()
GEOMETRIC_REPRESENTATION_ITEM()
RATIONAL_B_SPLINE_CURVE((1.02428162962097,1.02311336089458,1.02147610369991))
REPRESENTATION_ITEM('')
);
#437=(
BOUNDED_CURVE()
B_SPLINE_CURVE(2,(#35195,#35196,#35197),.UNSPECIFIED.,.F.,.F.)
B_SPLINE_CURVE_WITH_KNOTS((3,3),(-0.589144372850594,-0.536094506482411),
 .UNSPECIFIED.)
CURVE()
GEOMETRIC_REPRESENTATION_ITEM()
RATIONAL_B_SPLINE_CURVE((1.02147610369989,1.02311336089456,1.02428162962095))
REPRESENTATION_ITEM('')
);
#438=(
BOUNDED_CURVE()
B_SPLINE_CURVE(2,(#35201,#35202,#35203),.UNSPECIFIED.,.F.,.F.)
B_SPLINE_CURVE_WITH_KNOTS((3,3),(-0.271795897845358,-0.218746031477177),
 .UNSPECIFIED.)
CURVE()
GEOMETRIC_REPRESENTATION_ITEM()
RATIONAL_B_SPLINE_CURVE((1.02428162962088,1.0231133608945,1.02147610369983))
REPRESENTATION_ITEM('')
);
#439=(
BOUNDED_CURVE()
B_SPLINE_CURVE(2,(#35205,#35206,#35207),.UNSPECIFIED.,.F.,.F.)
B_SPLINE_CURVE_WITH_KNOTS((3,3),(-0.589144372850591,-0.536094506482403),
 .UNSPECIFIED.)
CURVE()
GEOMETRIC_REPRESENTATION_ITEM()
RATIONAL_B_SPLINE_CURVE((1.02147610369996,1.02311336089463,1.02428162962103))
REPRESENTATION_ITEM('')
);
#440=(
BOUNDED_CURVE()
B_SPLINE_CURVE(2,(#35211,#35212,#35213),.UNSPECIFIED.,.F.,.F.)
B_SPLINE_CURVE_WITH_KNOTS((3,3),(-0.271795897845352,-0.218746031477168),
 .UNSPECIFIED.)
CURVE()
GEOMETRIC_REPRESENTATION_ITEM()
RATIONAL_B_SPLINE_CURVE((1.02428162962098,1.02311336089459,1.02147610369992))
REPRESENTATION_ITEM('')
);
#441=(
BOUNDED_CURVE()
B_SPLINE_CURVE(2,(#35215,#35216,#35217),.UNSPECIFIED.,.F.,.F.)
B_SPLINE_CURVE_WITH_KNOTS((3,3),(-0.589144372850591,-0.536094506482408),
 .UNSPECIFIED.)
CURVE()
GEOMETRIC_REPRESENTATION_ITEM()
RATIONAL_B_SPLINE_CURVE((1.02147610369988,1.02311336089455,1.02428162962094))
REPRESENTATION_ITEM('')
);
#442=(
BOUNDED_CURVE()
B_SPLINE_CURVE(2,(#35221,#35222,#35223),.UNSPECIFIED.,.F.,.F.)
B_SPLINE_CURVE_WITH_KNOTS((3,3),(-0.271795897845345,-0.21874603147716),
 .UNSPECIFIED.)
CURVE()
GEOMETRIC_REPRESENTATION_ITEM()
RATIONAL_B_SPLINE_CURVE((1.024281629621,1.02311336089461,1.02147610369993))
REPRESENTATION_ITEM('')
);
#443=(
BOUNDED_CURVE()
B_SPLINE_CURVE(2,(#35225,#35226,#35227),.UNSPECIFIED.,.F.,.F.)
B_SPLINE_CURVE_WITH_KNOTS((3,3),(-0.589144372850594,-0.536094506482409),
 .UNSPECIFIED.)
CURVE()
GEOMETRIC_REPRESENTATION_ITEM()
RATIONAL_B_SPLINE_CURVE((1.02147610369992,1.02311336089459,1.02428162962098))
REPRESENTATION_ITEM('')
);
#444=(
BOUNDED_CURVE()
B_SPLINE_CURVE(2,(#35231,#35232,#35233),.UNSPECIFIED.,.F.,.F.)
B_SPLINE_CURVE_WITH_KNOTS((3,3),(-0.271795897845346,-0.218746031477163),
 .UNSPECIFIED.)
CURVE()
GEOMETRIC_REPRESENTATION_ITEM()
RATIONAL_B_SPLINE_CURVE((1.02428162962097,1.02311336089458,1.02147610369991))
REPRESENTATION_ITEM('')
);
#445=(
BOUNDED_CURVE()
B_SPLINE_CURVE(2,(#35235,#35236,#35237),.UNSPECIFIED.,.F.,.F.)
B_SPLINE_CURVE_WITH_KNOTS((3,3),(-0.589144372850596,-0.536094506482413),
 .UNSPECIFIED.)
CURVE()
GEOMETRIC_REPRESENTATION_ITEM()
RATIONAL_B_SPLINE_CURVE((1.02147610369989,1.02311336089456,1.02428162962095))
REPRESENTATION_ITEM('')
);
#446=(
BOUNDED_CURVE()
B_SPLINE_CURVE(2,(#35241,#35242,#35243),.UNSPECIFIED.,.F.,.F.)
B_SPLINE_CURVE_WITH_KNOTS((3,3),(-0.271795897845354,-0.218746031477172),
 .UNSPECIFIED.)
CURVE()
GEOMETRIC_REPRESENTATION_ITEM()
RATIONAL_B_SPLINE_CURVE((1.02428162962092,1.02311336089453,1.02147610369987))
REPRESENTATION_ITEM('')
);
#447=(
BOUNDED_CURVE()
B_SPLINE_CURVE(2,(#35245,#35246,#35247),.UNSPECIFIED.,.F.,.F.)
B_SPLINE_CURVE_WITH_KNOTS((3,3),(-0.589144372850593,-0.53609450648241),
 .UNSPECIFIED.)
CURVE()
GEOMETRIC_REPRESENTATION_ITEM()
RATIONAL_B_SPLINE_CURVE((1.02147610369989,1.02311336089456,1.02428162962095))
REPRESENTATION_ITEM('')
);
#448=(
BOUNDED_CURVE()
B_SPLINE_CURVE(2,(#35251,#35252,#35253),.UNSPECIFIED.,.F.,.F.)
B_SPLINE_CURVE_WITH_KNOTS((3,3),(-0.271795897845358,-0.218746031477176),
 .UNSPECIFIED.)
CURVE()
GEOMETRIC_REPRESENTATION_ITEM()
RATIONAL_B_SPLINE_CURVE((1.02428162962091,1.02311336089452,1.02147610369985))
REPRESENTATION_ITEM('')
);
#449=(
BOUNDED_CURVE()
B_SPLINE_CURVE(2,(#35255,#35256,#35257),.UNSPECIFIED.,.F.,.F.)
B_SPLINE_CURVE_WITH_KNOTS((3,3),(-0.589144372850596,-0.536094506482412),
 .UNSPECIFIED.)
CURVE()
GEOMETRIC_REPRESENTATION_ITEM()
RATIONAL_B_SPLINE_CURVE((1.02147610369988,1.02311336089455,1.02428162962094))
REPRESENTATION_ITEM('')
);
#450=(
BOUNDED_CURVE()
B_SPLINE_CURVE(2,(#35261,#35262,#35263),.UNSPECIFIED.,.F.,.F.)
B_SPLINE_CURVE_WITH_KNOTS((3,3),(-0.271795897845353,-0.218746031477168),
 .UNSPECIFIED.)
CURVE()
GEOMETRIC_REPRESENTATION_ITEM()
RATIONAL_B_SPLINE_CURVE((1.024281629621,1.02311336089461,1.02147610369994))
REPRESENTATION_ITEM('')
);
#451=(
BOUNDED_CURVE()
B_SPLINE_CURVE(2,(#35265,#35266,#35267),.UNSPECIFIED.,.F.,.F.)
B_SPLINE_CURVE_WITH_KNOTS((3,3),(-0.589144372850586,-0.536094506482402),
 .UNSPECIFIED.)
CURVE()
GEOMETRIC_REPRESENTATION_ITEM()
RATIONAL_B_SPLINE_CURVE((1.02147610369992,1.02311336089459,1.02428162962098))
REPRESENTATION_ITEM('')
);
#452=(
BOUNDED_CURVE()
B_SPLINE_CURVE(2,(#35271,#35272,#35273),.UNSPECIFIED.,.F.,.F.)
B_SPLINE_CURVE_WITH_KNOTS((3,3),(-0.271795897845356,-0.218746031477171),
 .UNSPECIFIED.)
CURVE()
GEOMETRIC_REPRESENTATION_ITEM()
RATIONAL_B_SPLINE_CURVE((1.02428162962097,1.02311336089458,1.0214761036999))
REPRESENTATION_ITEM('')
);
#453=(
BOUNDED_CURVE()
B_SPLINE_CURVE(2,(#35275,#35276,#35277),.UNSPECIFIED.,.F.,.F.)
B_SPLINE_CURVE_WITH_KNOTS((3,3),(-0.589144372850589,-0.536094506482406),
 .UNSPECIFIED.)
CURVE()
GEOMETRIC_REPRESENTATION_ITEM()
RATIONAL_B_SPLINE_CURVE((1.02147610369989,1.02311336089456,1.02428162962095))
REPRESENTATION_ITEM('')
);
#454=(
BOUNDED_CURVE()
B_SPLINE_CURVE(2,(#35281,#35282,#35283),.UNSPECIFIED.,.F.,.F.)
B_SPLINE_CURVE_WITH_KNOTS((3,3),(-0.271795897845358,-0.218746031477175),
 .UNSPECIFIED.)
CURVE()
GEOMETRIC_REPRESENTATION_ITEM()
RATIONAL_B_SPLINE_CURVE((1.02428162962095,1.02311336089456,1.02147610369989))
REPRESENTATION_ITEM('')
);
#455=(
BOUNDED_CURVE()
B_SPLINE_CURVE(2,(#35285,#35286,#35287),.UNSPECIFIED.,.F.,.F.)
B_SPLINE_CURVE_WITH_KNOTS((3,3),(-0.589144372850611,-0.536094506482426),
 .UNSPECIFIED.)
CURVE()
GEOMETRIC_REPRESENTATION_ITEM()
RATIONAL_B_SPLINE_CURVE((1.02147610369994,1.02311336089462,1.02428162962101))
REPRESENTATION_ITEM('')
);
#456=(
BOUNDED_CURVE()
B_SPLINE_CURVE(2,(#35291,#35292,#35293),.UNSPECIFIED.,.F.,.F.)
B_SPLINE_CURVE_WITH_KNOTS((3,3),(-0.271795897845356,-0.218746031477171),
 .UNSPECIFIED.)
CURVE()
GEOMETRIC_REPRESENTATION_ITEM()
RATIONAL_B_SPLINE_CURVE((1.02428162962099,1.0231133608946,1.02147610369993))
REPRESENTATION_ITEM('')
);
#457=(
BOUNDED_CURVE()
B_SPLINE_CURVE(2,(#35295,#35296,#35297),.UNSPECIFIED.,.F.,.F.)
B_SPLINE_CURVE_WITH_KNOTS((3,3),(-0.589144372850582,-0.536094506482403),
 .UNSPECIFIED.)
CURVE()
GEOMETRIC_REPRESENTATION_ITEM()
RATIONAL_B_SPLINE_CURVE((1.02147610369981,1.02311336089448,1.02428162962086))
REPRESENTATION_ITEM('')
);
#458=(
BOUNDED_CURVE()
B_SPLINE_CURVE(2,(#35301,#35302,#35303),.UNSPECIFIED.,.F.,.F.)
B_SPLINE_CURVE_WITH_KNOTS((3,3),(-0.271795897845348,-0.218746031477162),
 .UNSPECIFIED.)
CURVE()
GEOMETRIC_REPRESENTATION_ITEM()
RATIONAL_B_SPLINE_CURVE((1.02428162962101,1.02311336089462,1.02147610369994))
REPRESENTATION_ITEM('')
);
#459=(
BOUNDED_CURVE()
B_SPLINE_CURVE(2,(#35305,#35306,#35307),.UNSPECIFIED.,.F.,.F.)
B_SPLINE_CURVE_WITH_KNOTS((3,3),(-0.589144372850586,-0.536094506482406),
 .UNSPECIFIED.)
CURVE()
GEOMETRIC_REPRESENTATION_ITEM()
RATIONAL_B_SPLINE_CURVE((1.02147610369985,1.02311336089452,1.02428162962091))
REPRESENTATION_ITEM('')
);
#460=(
BOUNDED_CURVE()
B_SPLINE_CURVE(2,(#35311,#35312,#35313),.UNSPECIFIED.,.F.,.F.)
B_SPLINE_CURVE_WITH_KNOTS((3,3),(-0.271795897845348,-0.218746031477166),
 .UNSPECIFIED.)
CURVE()
GEOMETRIC_REPRESENTATION_ITEM()
RATIONAL_B_SPLINE_CURVE((1.02428162962094,1.02311336089455,1.02147610369988))
REPRESENTATION_ITEM('')
);
#461=(
BOUNDED_CURVE()
B_SPLINE_CURVE(2,(#35315,#35316,#35317),.UNSPECIFIED.,.F.,.F.)
B_SPLINE_CURVE_WITH_KNOTS((3,3),(-0.589144372850589,-0.536094506482402),
 .UNSPECIFIED.)
CURVE()
GEOMETRIC_REPRESENTATION_ITEM()
RATIONAL_B_SPLINE_CURVE((1.02147610369993,1.0231133608946,1.02428162962099))
REPRESENTATION_ITEM('')
);
#462=(
BOUNDED_CURVE()
B_SPLINE_CURVE(2,(#35321,#35322,#35323),.UNSPECIFIED.,.F.,.F.)
B_SPLINE_CURVE_WITH_KNOTS((3,3),(-0.271795897845359,-0.218746031477172),
 .UNSPECIFIED.)
CURVE()
GEOMETRIC_REPRESENTATION_ITEM()
RATIONAL_B_SPLINE_CURVE((1.02428162962103,1.02311336089464,1.02147610369996))
REPRESENTATION_ITEM('')
);
#463=(
BOUNDED_CURVE()
B_SPLINE_CURVE(2,(#35325,#35326,#35327),.UNSPECIFIED.,.F.,.F.)
B_SPLINE_CURVE_WITH_KNOTS((3,3),(-0.589144372850584,-0.536094506482398),
 .UNSPECIFIED.)
CURVE()
GEOMETRIC_REPRESENTATION_ITEM()
RATIONAL_B_SPLINE_CURVE((1.02147610369995,1.02311336089463,1.02428162962102))
REPRESENTATION_ITEM('')
);
#464=(
BOUNDED_CURVE()
B_SPLINE_CURVE(2,(#35331,#35332,#35333),.UNSPECIFIED.,.F.,.F.)
B_SPLINE_CURVE_WITH_KNOTS((3,3),(-0.271795897845344,-0.218746031477162),
 .UNSPECIFIED.)
CURVE()
GEOMETRIC_REPRESENTATION_ITEM()
RATIONAL_B_SPLINE_CURVE((1.02428162962092,1.02311336089454,1.02147610369987))
REPRESENTATION_ITEM('')
);
#465=(
BOUNDED_CURVE()
B_SPLINE_CURVE(2,(#35335,#35336,#35337),.UNSPECIFIED.,.F.,.F.)
B_SPLINE_CURVE_WITH_KNOTS((3,3),(-0.589144372850587,-0.536094506482403),
 .UNSPECIFIED.)
CURVE()
GEOMETRIC_REPRESENTATION_ITEM()
RATIONAL_B_SPLINE_CURVE((1.0214761036999,1.02311336089457,1.02428162962096))
REPRESENTATION_ITEM('')
);
#466=(
BOUNDED_CURVE()
B_SPLINE_CURVE(2,(#35341,#35342,#35343),.UNSPECIFIED.,.F.,.F.)
B_SPLINE_CURVE_WITH_KNOTS((3,3),(-0.27179589784536,-0.218746031477177),
 .UNSPECIFIED.)
CURVE()
GEOMETRIC_REPRESENTATION_ITEM()
RATIONAL_B_SPLINE_CURVE((1.02428162962093,1.02311336089455,1.02147610369988))
REPRESENTATION_ITEM('')
);
#467=(
BOUNDED_CURVE()
B_SPLINE_CURVE(2,(#35345,#35346,#35347),.UNSPECIFIED.,.F.,.F.)
B_SPLINE_CURVE_WITH_KNOTS((3,3),(-0.589144372850582,-0.536094506482399),
 .UNSPECIFIED.)
CURVE()
GEOMETRIC_REPRESENTATION_ITEM()
RATIONAL_B_SPLINE_CURVE((1.02147610369987,1.02311336089454,1.02428162962092))
REPRESENTATION_ITEM('')
);
#468=(
BOUNDED_CURVE()
B_SPLINE_CURVE(2,(#35351,#35352,#35353),.UNSPECIFIED.,.F.,.F.)
B_SPLINE_CURVE_WITH_KNOTS((3,3),(-0.27179589784536,-0.21874603147718),
 .UNSPECIFIED.)
CURVE()
GEOMETRIC_REPRESENTATION_ITEM()
RATIONAL_B_SPLINE_CURVE((1.02428162962089,1.0231133608945,1.02147610369983))
REPRESENTATION_ITEM('')
);
#469=(
BOUNDED_CURVE()
B_SPLINE_CURVE(2,(#35355,#35356,#35357),.UNSPECIFIED.,.F.,.F.)
B_SPLINE_CURVE_WITH_KNOTS((3,3),(-0.589144372850591,-0.536094506482404),
 .UNSPECIFIED.)
CURVE()
GEOMETRIC_REPRESENTATION_ITEM()
RATIONAL_B_SPLINE_CURVE((1.02147610369995,1.02311336089462,1.02428162962101))
REPRESENTATION_ITEM('')
);
#470=(
BOUNDED_CURVE()
B_SPLINE_CURVE(2,(#35361,#35362,#35363),.UNSPECIFIED.,.F.,.F.)
B_SPLINE_CURVE_WITH_KNOTS((3,3),(-0.271795897845354,-0.21874603147717),
 .UNSPECIFIED.)
CURVE()
GEOMETRIC_REPRESENTATION_ITEM()
RATIONAL_B_SPLINE_CURVE((1.02428162962096,1.02311336089457,1.0214761036999))
REPRESENTATION_ITEM('')
);
#471=(
BOUNDED_CURVE()
B_SPLINE_CURVE(2,(#35365,#35366,#35367),.UNSPECIFIED.,.F.,.F.)
B_SPLINE_CURVE_WITH_KNOTS((3,3),(-0.58914437285059,-0.536094506482403),
 .UNSPECIFIED.)
CURVE()
GEOMETRIC_REPRESENTATION_ITEM()
RATIONAL_B_SPLINE_CURVE((1.02147610369995,1.02311336089463,1.02428162962102))
REPRESENTATION_ITEM('')
);
#472=(
BOUNDED_CURVE()
B_SPLINE_CURVE(2,(#35371,#35372,#35373),.UNSPECIFIED.,.F.,.F.)
B_SPLINE_CURVE_WITH_KNOTS((3,3),(-0.271795897845357,-0.218746031477171),
 .UNSPECIFIED.)
CURVE()
GEOMETRIC_REPRESENTATION_ITEM()
RATIONAL_B_SPLINE_CURVE((1.024281629621,1.02311336089461,1.02147610369993))
REPRESENTATION_ITEM('')
);
#473=(
BOUNDED_CURVE()
B_SPLINE_CURVE(2,(#35375,#35376,#35377),.UNSPECIFIED.,.F.,.F.)
B_SPLINE_CURVE_WITH_KNOTS((3,3),(-0.589144372850596,-0.536094506482413),
 .UNSPECIFIED.)
CURVE()
GEOMETRIC_REPRESENTATION_ITEM()
RATIONAL_B_SPLINE_CURVE((1.02147610369988,1.02311336089455,1.02428162962094))
REPRESENTATION_ITEM('')
);
#474=(
BOUNDED_CURVE()
B_SPLINE_CURVE(2,(#35381,#35382,#35383),.UNSPECIFIED.,.F.,.F.)
B_SPLINE_CURVE_WITH_KNOTS((3,3),(-0.27179589784535,-0.270098893534619),
 .UNSPECIFIED.)
CURVE()
GEOMETRIC_REPRESENTATION_ITEM()
RATIONAL_B_SPLINE_CURVE((1.02428162962103,1.02424425804593,1.02420640656121))
REPRESENTATION_ITEM('')
);
#475=(
BOUNDED_CURVE()
B_SPLINE_CURVE(2,(#35388,#35389,#35390),.UNSPECIFIED.,.F.,.F.)
B_SPLINE_CURVE_WITH_KNOTS((3,3),(-0.270098893534619,-0.218746031477162),
 .UNSPECIFIED.)
CURVE()
GEOMETRIC_REPRESENTATION_ITEM()
RATIONAL_B_SPLINE_CURVE((1.02420640656121,1.02306098691696,1.02147610369996))
REPRESENTATION_ITEM('')
);
#476=(
BOUNDED_CURVE()
B_SPLINE_CURVE(2,(#35392,#35393,#35394),.UNSPECIFIED.,.F.,.F.)
B_SPLINE_CURVE_WITH_KNOTS((3,3),(-0.589144372850598,-0.536094506482416),
 .UNSPECIFIED.)
CURVE()
GEOMETRIC_REPRESENTATION_ITEM()
RATIONAL_B_SPLINE_CURVE((1.02147610369987,1.02311336089454,1.02428162962093))
REPRESENTATION_ITEM('')
);
#477=(
BOUNDED_CURVE()
B_SPLINE_CURVE(2,(#35398,#35399,#35400),.UNSPECIFIED.,.F.,.F.)
B_SPLINE_CURVE_WITH_KNOTS((3,3),(-0.271795897845349,-0.218746031477166),
 .UNSPECIFIED.)
CURVE()
GEOMETRIC_REPRESENTATION_ITEM()
RATIONAL_B_SPLINE_CURVE((1.02428162962097,1.02311336089458,1.02147610369991))
REPRESENTATION_ITEM('')
);
#478=(
BOUNDED_CURVE()
B_SPLINE_CURVE(2,(#35402,#35403,#35404),.UNSPECIFIED.,.F.,.F.)
B_SPLINE_CURVE_WITH_KNOTS((3,3),(-0.589144372850578,-0.536094506482394),
 .UNSPECIFIED.)
CURVE()
GEOMETRIC_REPRESENTATION_ITEM()
RATIONAL_B_SPLINE_CURVE((1.02147610369988,1.02311336089455,1.02428162962093))
REPRESENTATION_ITEM('')
);
#479=(
BOUNDED_CURVE()
B_SPLINE_CURVE(2,(#35408,#35409,#35410),.UNSPECIFIED.,.F.,.F.)
B_SPLINE_CURVE_WITH_KNOTS((3,3),(-0.27179589784536,-0.218746031477173),
 .UNSPECIFIED.)
CURVE()
GEOMETRIC_REPRESENTATION_ITEM()
RATIONAL_B_SPLINE_CURVE((1.024281629621,1.02311336089461,1.02147610369993))
REPRESENTATION_ITEM('')
);
#480=(
BOUNDED_CURVE()
B_SPLINE_CURVE(2,(#35412,#35413,#35414),.UNSPECIFIED.,.F.,.F.)
B_SPLINE_CURVE_WITH_KNOTS((3,3),(-0.589144372850572,-0.536094506482391),
 .UNSPECIFIED.)
CURVE()
GEOMETRIC_REPRESENTATION_ITEM()
RATIONAL_B_SPLINE_CURVE((1.02147610369982,1.02311336089448,1.02428162962086))
REPRESENTATION_ITEM('')
);
#481=(
BOUNDED_CURVE()
B_SPLINE_CURVE(2,(#35418,#35419,#35420),.UNSPECIFIED.,.F.,.F.)
B_SPLINE_CURVE_WITH_KNOTS((3,3),(-0.271795897845356,-0.21874603147717),
 .UNSPECIFIED.)
CURVE()
GEOMETRIC_REPRESENTATION_ITEM()
RATIONAL_B_SPLINE_CURVE((1.02428162962099,1.0231133608946,1.02147610369993))
REPRESENTATION_ITEM('')
);
#482=(
BOUNDED_CURVE()
B_SPLINE_CURVE(2,(#35422,#35423,#35424),.UNSPECIFIED.,.F.,.F.)
B_SPLINE_CURVE_WITH_KNOTS((3,3),(-0.589144372850566,-0.536094506482389),
 .UNSPECIFIED.)
CURVE()
GEOMETRIC_REPRESENTATION_ITEM()
RATIONAL_B_SPLINE_CURVE((1.02147610369972,1.02311336089438,1.02428162962076))
REPRESENTATION_ITEM('')
);
#483=(
BOUNDED_CURVE()
B_SPLINE_CURVE(2,(#35428,#35429,#35430),.UNSPECIFIED.,.F.,.F.)
B_SPLINE_CURVE_WITH_KNOTS((3,3),(-0.271795897845343,-0.218746031477157),
 .UNSPECIFIED.)
CURVE()
GEOMETRIC_REPRESENTATION_ITEM()
RATIONAL_B_SPLINE_CURVE((1.02428162962101,1.02311336089462,1.02147610369994))
REPRESENTATION_ITEM('')
);
#484=(
BOUNDED_CURVE()
B_SPLINE_CURVE(2,(#35432,#35433,#35434),.UNSPECIFIED.,.F.,.F.)
B_SPLINE_CURVE_WITH_KNOTS((3,3),(-0.589144372850584,-0.536094506482395),
 .UNSPECIFIED.)
CURVE()
GEOMETRIC_REPRESENTATION_ITEM()
RATIONAL_B_SPLINE_CURVE((1.02147610369997,1.02311336089465,1.02428162962104))
REPRESENTATION_ITEM('')
);
#485=(
BOUNDED_CURVE()
B_SPLINE_CURVE(2,(#35438,#35439,#35440),.UNSPECIFIED.,.F.,.F.)
B_SPLINE_CURVE_WITH_KNOTS((3,3),(-0.27179589784534,-0.218746031477154),
 .UNSPECIFIED.)
CURVE()
GEOMETRIC_REPRESENTATION_ITEM()
RATIONAL_B_SPLINE_CURVE((1.02428162962103,1.02311336089464,1.02147610369996))
REPRESENTATION_ITEM('')
);
#486=(
BOUNDED_CURVE()
B_SPLINE_CURVE(2,(#35442,#35443,#35444),.UNSPECIFIED.,.F.,.F.)
B_SPLINE_CURVE_WITH_KNOTS((3,3),(-0.589144372850587,-0.536094506482399),
 .UNSPECIFIED.)
CURVE()
GEOMETRIC_REPRESENTATION_ITEM()
RATIONAL_B_SPLINE_CURVE((1.02147610369995,1.02311336089463,1.02428162962102))
REPRESENTATION_ITEM('')
);
#487=(
BOUNDED_CURVE()
B_SPLINE_CURVE(2,(#35448,#35449,#35450),.UNSPECIFIED.,.F.,.F.)
B_SPLINE_CURVE_WITH_KNOTS((3,3),(-0.271795897845355,-0.218746031477173),
 .UNSPECIFIED.)
CURVE()
GEOMETRIC_REPRESENTATION_ITEM()
RATIONAL_B_SPLINE_CURVE((1.02428162962092,1.02311336089454,1.02147610369987))
REPRESENTATION_ITEM('')
);
#488=(
BOUNDED_CURVE()
B_SPLINE_CURVE(2,(#35452,#35453,#35454),.UNSPECIFIED.,.F.,.F.)
B_SPLINE_CURVE_WITH_KNOTS((3,3),(-0.58914437285059,-0.536094506482405),
 .UNSPECIFIED.)
CURVE()
GEOMETRIC_REPRESENTATION_ITEM()
RATIONAL_B_SPLINE_CURVE((1.02147610369994,1.02311336089462,1.02428162962101))
REPRESENTATION_ITEM('')
);
#489=(
BOUNDED_CURVE()
B_SPLINE_CURVE(2,(#35458,#35459,#35460),.UNSPECIFIED.,.F.,.F.)
B_SPLINE_CURVE_WITH_KNOTS((3,3),(-0.271795897845348,-0.218746031477163),
 .UNSPECIFIED.)
CURVE()
GEOMETRIC_REPRESENTATION_ITEM()
RATIONAL_B_SPLINE_CURVE((1.02428162962098,1.02311336089459,1.02147610369992))
REPRESENTATION_ITEM('')
);
#490=(
BOUNDED_CURVE()
B_SPLINE_CURVE(2,(#35462,#35463,#35464),.UNSPECIFIED.,.F.,.F.)
B_SPLINE_CURVE_WITH_KNOTS((3,3),(-0.589144372850584,-0.536094506482403),
 .UNSPECIFIED.)
CURVE()
GEOMETRIC_REPRESENTATION_ITEM()
RATIONAL_B_SPLINE_CURVE((1.02147610369983,1.0231133608945,1.02428162962088))
REPRESENTATION_ITEM('')
);
#491=(
BOUNDED_CURVE()
B_SPLINE_CURVE(2,(#35468,#35469,#35470),.UNSPECIFIED.,.F.,.F.)
B_SPLINE_CURVE_WITH_KNOTS((3,3),(-0.27179589784536,-0.218746031477177),
 .UNSPECIFIED.)
CURVE()
GEOMETRIC_REPRESENTATION_ITEM()
RATIONAL_B_SPLINE_CURVE((1.02428162962094,1.02311336089455,1.02147610369988))
REPRESENTATION_ITEM('')
);
#492=(
BOUNDED_CURVE()
B_SPLINE_CURVE(2,(#35472,#35473,#35474),.UNSPECIFIED.,.F.,.F.)
B_SPLINE_CURVE_WITH_KNOTS((3,3),(-0.589144372850591,-0.536094506482406),
 .UNSPECIFIED.)
CURVE()
GEOMETRIC_REPRESENTATION_ITEM()
RATIONAL_B_SPLINE_CURVE((1.02147610369995,1.02311336089463,1.02428162962102))
REPRESENTATION_ITEM('')
);
#493=(
BOUNDED_CURVE()
B_SPLINE_CURVE(2,(#35478,#35479,#35480),.UNSPECIFIED.,.F.,.F.)
B_SPLINE_CURVE_WITH_KNOTS((3,3),(-0.271795897845357,-0.218746031477177),
 .UNSPECIFIED.)
CURVE()
GEOMETRIC_REPRESENTATION_ITEM()
RATIONAL_B_SPLINE_CURVE((1.02428162962087,1.02311336089449,1.02147610369982))
REPRESENTATION_ITEM('')
);
#494=(
BOUNDED_CURVE()
B_SPLINE_CURVE(2,(#35482,#35483,#35484),.UNSPECIFIED.,.F.,.F.)
B_SPLINE_CURVE_WITH_KNOTS((3,3),(-0.589144372850584,-0.536094506482401),
 .UNSPECIFIED.)
CURVE()
GEOMETRIC_REPRESENTATION_ITEM()
RATIONAL_B_SPLINE_CURVE((1.02147610369986,1.02311336089452,1.02428162962091))
REPRESENTATION_ITEM('')
);
#495=(
BOUNDED_CURVE()
B_SPLINE_CURVE(2,(#35488,#35489,#35490),.UNSPECIFIED.,.F.,.F.)
B_SPLINE_CURVE_WITH_KNOTS((3,3),(-0.27179589784536,-0.21874603147717),
 .UNSPECIFIED.)
CURVE()
GEOMETRIC_REPRESENTATION_ITEM()
RATIONAL_B_SPLINE_CURVE((1.02428162962108,1.02311336089468,1.0214761037))
REPRESENTATION_ITEM('')
);
#496=(
BOUNDED_CURVE()
B_SPLINE_CURVE(2,(#35492,#35493,#35494),.UNSPECIFIED.,.F.,.F.)
B_SPLINE_CURVE_WITH_KNOTS((3,3),(-0.589144372850587,-0.536094506482401),
 .UNSPECIFIED.)
CURVE()
GEOMETRIC_REPRESENTATION_ITEM()
RATIONAL_B_SPLINE_CURVE((1.02147610369992,1.02311336089459,1.02428162962098))
REPRESENTATION_ITEM('')
);
#497=(
BOUNDED_CURVE()
B_SPLINE_CURVE(2,(#35498,#35499,#35500),.UNSPECIFIED.,.F.,.F.)
B_SPLINE_CURVE_WITH_KNOTS((3,3),(-0.271795897845351,-0.218746031477167),
 .UNSPECIFIED.)
CURVE()
GEOMETRIC_REPRESENTATION_ITEM()
RATIONAL_B_SPLINE_CURVE((1.02428162962096,1.02311336089457,1.0214761036999))
REPRESENTATION_ITEM('')
);
#498=(
BOUNDED_CURVE()
B_SPLINE_CURVE(2,(#35502,#35503,#35504),.UNSPECIFIED.,.F.,.F.)
B_SPLINE_CURVE_WITH_KNOTS((3,3),(-0.589144372850593,-0.53609450648241),
 .UNSPECIFIED.)
CURVE()
GEOMETRIC_REPRESENTATION_ITEM()
RATIONAL_B_SPLINE_CURVE((1.02147610369987,1.02311336089454,1.02428162962093))
REPRESENTATION_ITEM('')
);
#499=(
BOUNDED_CURVE()
B_SPLINE_CURVE(2,(#35508,#35509,#35510),.UNSPECIFIED.,.F.,.F.)
B_SPLINE_CURVE_WITH_KNOTS((3,3),(-0.271795897845359,-0.218746031477174),
 .UNSPECIFIED.)
CURVE()
GEOMETRIC_REPRESENTATION_ITEM()
RATIONAL_B_SPLINE_CURVE((1.02428162962098,1.02311336089459,1.02147610369992))
REPRESENTATION_ITEM('')
);
#500=(
BOUNDED_CURVE()
B_SPLINE_CURVE(2,(#35512,#35513,#35514),.UNSPECIFIED.,.F.,.F.)
B_SPLINE_CURVE_WITH_KNOTS((3,3),(-0.589144372850586,-0.536094506482401),
 .UNSPECIFIED.)
CURVE()
GEOMETRIC_REPRESENTATION_ITEM()
RATIONAL_B_SPLINE_CURVE((1.02147610369989,1.02311336089456,1.02428162962095))
REPRESENTATION_ITEM('')
);
#501=(
BOUNDED_CURVE()
B_SPLINE_CURVE(2,(#35518,#35519,#35520),.UNSPECIFIED.,.F.,.F.)
B_SPLINE_CURVE_WITH_KNOTS((3,3),(-0.271795897845355,-0.218746031477172),
 .UNSPECIFIED.)
CURVE()
GEOMETRIC_REPRESENTATION_ITEM()
RATIONAL_B_SPLINE_CURVE((1.02428162962095,1.02311336089456,1.02147610369989))
REPRESENTATION_ITEM('')
);
#502=(
BOUNDED_CURVE()
B_SPLINE_CURVE(2,(#35522,#35523,#35524),.UNSPECIFIED.,.F.,.F.)
B_SPLINE_CURVE_WITH_KNOTS((3,3),(-0.589144372850602,-0.536094506482415),
 .UNSPECIFIED.)
CURVE()
GEOMETRIC_REPRESENTATION_ITEM()
RATIONAL_B_SPLINE_CURVE((1.02147610369999,1.02311336089467,1.02428162962106))
REPRESENTATION_ITEM('')
);
#503=(
BOUNDED_CURVE()
B_SPLINE_CURVE(2,(#35528,#35529,#35530),.UNSPECIFIED.,.F.,.F.)
B_SPLINE_CURVE_WITH_KNOTS((3,3),(-0.271795897845356,-0.218746031477167),
 .UNSPECIFIED.)
CURVE()
GEOMETRIC_REPRESENTATION_ITEM()
RATIONAL_B_SPLINE_CURVE((1.02428162962107,1.02311336089467,1.02147610369999))
REPRESENTATION_ITEM('')
);
#504=(
BOUNDED_CURVE()
B_SPLINE_CURVE(2,(#35532,#35533,#35534),.UNSPECIFIED.,.F.,.F.)
B_SPLINE_CURVE_WITH_KNOTS((3,3),(-0.589144372850598,-0.53609450648241),
 .UNSPECIFIED.)
CURVE()
GEOMETRIC_REPRESENTATION_ITEM()
RATIONAL_B_SPLINE_CURVE((1.02147610369999,1.02311336089467,1.02428162962106))
REPRESENTATION_ITEM('')
);
#505=(
BOUNDED_CURVE()
B_SPLINE_CURVE(2,(#35538,#35539,#35540),.UNSPECIFIED.,.F.,.F.)
B_SPLINE_CURVE_WITH_KNOTS((3,3),(-0.271795897845352,-0.218746031477168),
 .UNSPECIFIED.)
CURVE()
GEOMETRIC_REPRESENTATION_ITEM()
RATIONAL_B_SPLINE_CURVE((1.02428162962095,1.02311336089457,1.02147610369989))
REPRESENTATION_ITEM('')
);
#506=(
BOUNDED_CURVE()
B_SPLINE_CURVE(2,(#35542,#35543,#35544),.UNSPECIFIED.,.F.,.F.)
B_SPLINE_CURVE_WITH_KNOTS((3,3),(-0.5891443728506,-0.536094506482413),
 .UNSPECIFIED.)
CURVE()
GEOMETRIC_REPRESENTATION_ITEM()
RATIONAL_B_SPLINE_CURVE((1.02147610369997,1.02311336089465,1.02428162962104))
REPRESENTATION_ITEM('')
);
#507=(
BOUNDED_CURVE()
B_SPLINE_CURVE(2,(#35548,#35549,#35550),.UNSPECIFIED.,.F.,.F.)
B_SPLINE_CURVE_WITH_KNOTS((3,3),(-0.271795897845352,-0.218746031477163),
 .UNSPECIFIED.)
CURVE()
GEOMETRIC_REPRESENTATION_ITEM()
RATIONAL_B_SPLINE_CURVE((1.02428162962108,1.02311336089468,1.0214761037))
REPRESENTATION_ITEM('')
);
#508=(
BOUNDED_CURVE()
B_SPLINE_CURVE(2,(#35552,#35553,#35554),.UNSPECIFIED.,.F.,.F.)
B_SPLINE_CURVE_WITH_KNOTS((3,3),(-0.589144372850592,-0.536094506482407),
 .UNSPECIFIED.)
CURVE()
GEOMETRIC_REPRESENTATION_ITEM()
RATIONAL_B_SPLINE_CURVE((1.02147610369993,1.0231133608946,1.02428162962099))
REPRESENTATION_ITEM('')
);
#509=(
BOUNDED_CURVE()
B_SPLINE_CURVE(2,(#35558,#35559,#35560),.UNSPECIFIED.,.F.,.F.)
B_SPLINE_CURVE_WITH_KNOTS((3,3),(-0.271795897845362,-0.218746031477183),
 .UNSPECIFIED.)
CURVE()
GEOMETRIC_REPRESENTATION_ITEM()
RATIONAL_B_SPLINE_CURVE((1.02428162962086,1.02311336089448,1.02147610369982))
REPRESENTATION_ITEM('')
);
#510=(
BOUNDED_CURVE()
B_SPLINE_CURVE(2,(#35562,#35563,#35564),.UNSPECIFIED.,.F.,.F.)
B_SPLINE_CURVE_WITH_KNOTS((3,3),(-0.589144372850588,-0.536094506482407),
 .UNSPECIFIED.)
CURVE()
GEOMETRIC_REPRESENTATION_ITEM()
RATIONAL_B_SPLINE_CURVE((1.02147610369984,1.0231133608945,1.02428162962089))
REPRESENTATION_ITEM('')
);
#511=(
BOUNDED_CURVE()
B_SPLINE_CURVE(2,(#35568,#35569,#35570),.UNSPECIFIED.,.F.,.F.)
B_SPLINE_CURVE_WITH_KNOTS((3,3),(-0.271795897845349,-0.218746031477166),
 .UNSPECIFIED.)
CURVE()
GEOMETRIC_REPRESENTATION_ITEM()
RATIONAL_B_SPLINE_CURVE((1.02428162962096,1.02311336089457,1.0214761036999))
REPRESENTATION_ITEM('')
);
#512=(
BOUNDED_CURVE()
B_SPLINE_CURVE(2,(#35572,#35573,#35574),.UNSPECIFIED.,.F.,.F.)
B_SPLINE_CURVE_WITH_KNOTS((3,3),(-0.589144372850592,-0.536094506482409),
 .UNSPECIFIED.)
CURVE()
GEOMETRIC_REPRESENTATION_ITEM()
RATIONAL_B_SPLINE_CURVE((1.02147610369988,1.02311336089455,1.02428162962093))
REPRESENTATION_ITEM('')
);
#513=(
BOUNDED_CURVE()
B_SPLINE_CURVE(2,(#35578,#35579,#35580),.UNSPECIFIED.,.F.,.F.)
B_SPLINE_CURVE_WITH_KNOTS((3,3),(-0.271795897845356,-0.218746031477174),
 .UNSPECIFIED.)
CURVE()
GEOMETRIC_REPRESENTATION_ITEM()
RATIONAL_B_SPLINE_CURVE((1.0242816296209,1.02311336089451,1.02147610369985))
REPRESENTATION_ITEM('')
);
#514=(
BOUNDED_CURVE()
B_SPLINE_CURVE(2,(#35582,#35583,#35584),.UNSPECIFIED.,.F.,.F.)
B_SPLINE_CURVE_WITH_KNOTS((3,3),(-0.589144372850584,-0.536094506482399),
 .UNSPECIFIED.)
CURVE()
GEOMETRIC_REPRESENTATION_ITEM()
RATIONAL_B_SPLINE_CURVE((1.02147610369989,1.02311336089456,1.02428162962095))
REPRESENTATION_ITEM('')
);
#515=(
BOUNDED_CURVE()
B_SPLINE_CURVE(2,(#35588,#35589,#35590),.UNSPECIFIED.,.F.,.F.)
B_SPLINE_CURVE_WITH_KNOTS((3,3),(-0.271795897845347,-0.218746031477166),
 .UNSPECIFIED.)
CURVE()
GEOMETRIC_REPRESENTATION_ITEM()
RATIONAL_B_SPLINE_CURVE((1.02428162962092,1.02311336089453,1.02147610369987))
REPRESENTATION_ITEM('')
);
#516=(
BOUNDED_CURVE()
B_SPLINE_CURVE(2,(#35592,#35593,#35594),.UNSPECIFIED.,.F.,.F.)
B_SPLINE_CURVE_WITH_KNOTS((3,3),(-0.58914437285059,-0.536094506482399),
 .UNSPECIFIED.)
CURVE()
GEOMETRIC_REPRESENTATION_ITEM()
RATIONAL_B_SPLINE_CURVE((1.02147610370001,1.02311336089469,1.02428162962109))
REPRESENTATION_ITEM('')
);
#517=(
BOUNDED_CURVE()
B_SPLINE_CURVE(2,(#35598,#35599,#35600),.UNSPECIFIED.,.F.,.F.)
B_SPLINE_CURVE_WITH_KNOTS((3,3),(-0.271795897845344,-0.218746031477161),
 .UNSPECIFIED.)
CURVE()
GEOMETRIC_REPRESENTATION_ITEM()
RATIONAL_B_SPLINE_CURVE((1.02428162962097,1.02311336089458,1.02147610369991))
REPRESENTATION_ITEM('')
);
#518=(
BOUNDED_CURVE()
B_SPLINE_CURVE(2,(#35602,#35603,#35604),.UNSPECIFIED.,.F.,.F.)
B_SPLINE_CURVE_WITH_KNOTS((3,3),(-0.589144372850593,-0.536094506482405),
 .UNSPECIFIED.)
CURVE()
GEOMETRIC_REPRESENTATION_ITEM()
RATIONAL_B_SPLINE_CURVE((1.02147610369996,1.02311336089464,1.02428162962103))
REPRESENTATION_ITEM('')
);
#519=(
BOUNDED_CURVE()
B_SPLINE_CURVE(2,(#35608,#35609,#35610),.UNSPECIFIED.,.F.,.F.)
B_SPLINE_CURVE_WITH_KNOTS((3,3),(-0.271795897845349,-0.218746031477166),
 .UNSPECIFIED.)
CURVE()
GEOMETRIC_REPRESENTATION_ITEM()
RATIONAL_B_SPLINE_CURVE((1.02428162962095,1.02311336089457,1.02147610369989))
REPRESENTATION_ITEM('')
);
#520=(
BOUNDED_CURVE()
B_SPLINE_CURVE(2,(#35612,#35613,#35614),.UNSPECIFIED.,.F.,.F.)
B_SPLINE_CURVE_WITH_KNOTS((3,3),(-0.589144372850592,-0.536094506482407),
 .UNSPECIFIED.)
CURVE()
GEOMETRIC_REPRESENTATION_ITEM()
RATIONAL_B_SPLINE_CURVE((1.02147610369992,1.02311336089459,1.02428162962098))
REPRESENTATION_ITEM('')
);
#521=(
BOUNDED_CURVE()
B_SPLINE_CURVE(2,(#35618,#35619,#35620),.UNSPECIFIED.,.F.,.F.)
B_SPLINE_CURVE_WITH_KNOTS((3,3),(-0.271795897845362,-0.218746031477179),
 .UNSPECIFIED.)
CURVE()
GEOMETRIC_REPRESENTATION_ITEM()
RATIONAL_B_SPLINE_CURVE((1.02428162962093,1.02311336089454,1.02147610369987))
REPRESENTATION_ITEM('')
);
#522=(
BOUNDED_CURVE()
B_SPLINE_CURVE(2,(#35622,#35623,#35624),.UNSPECIFIED.,.F.,.F.)
B_SPLINE_CURVE_WITH_KNOTS((3,3),(-0.589144372850592,-0.536094506482405),
 .UNSPECIFIED.)
CURVE()
GEOMETRIC_REPRESENTATION_ITEM()
RATIONAL_B_SPLINE_CURVE((1.02147610369993,1.02311336089461,1.024281629621))
REPRESENTATION_ITEM('')
);
#523=(
BOUNDED_CURVE()
B_SPLINE_CURVE(2,(#35628,#35629,#35630),.UNSPECIFIED.,.F.,.F.)
B_SPLINE_CURVE_WITH_KNOTS((3,3),(-0.271795897845364,-0.218746031477179),
 .UNSPECIFIED.)
CURVE()
GEOMETRIC_REPRESENTATION_ITEM()
RATIONAL_B_SPLINE_CURVE((1.02428162962097,1.02311336089458,1.02147610369991))
REPRESENTATION_ITEM('')
);
#524=(
BOUNDED_CURVE()
B_SPLINE_CURVE(2,(#35632,#35633,#35634),.UNSPECIFIED.,.F.,.F.)
B_SPLINE_CURVE_WITH_KNOTS((3,3),(-0.589144372850588,-0.536094506482402),
 .UNSPECIFIED.)
CURVE()
GEOMETRIC_REPRESENTATION_ITEM()
RATIONAL_B_SPLINE_CURVE((1.02147610369993,1.0231133608946,1.02428162962099))
REPRESENTATION_ITEM('')
);
#525=(
BOUNDED_CURVE()
B_SPLINE_CURVE(2,(#35638,#35639,#35640),.UNSPECIFIED.,.F.,.F.)
B_SPLINE_CURVE_WITH_KNOTS((3,3),(-0.271795897845357,-0.218746031477173),
 .UNSPECIFIED.)
CURVE()
GEOMETRIC_REPRESENTATION_ITEM()
RATIONAL_B_SPLINE_CURVE((1.02428162962094,1.02311336089455,1.02147610369988))
REPRESENTATION_ITEM('')
);
#526=(
BOUNDED_CURVE()
B_SPLINE_CURVE(2,(#35642,#35643,#35644),.UNSPECIFIED.,.F.,.F.)
B_SPLINE_CURVE_WITH_KNOTS((3,3),(-0.589144372850606,-0.536094506482418),
 .UNSPECIFIED.)
CURVE()
GEOMETRIC_REPRESENTATION_ITEM()
RATIONAL_B_SPLINE_CURVE((1.02147610369999,1.02311336089467,1.02428162962107))
REPRESENTATION_ITEM('')
);
#527=(
BOUNDED_CURVE()
B_SPLINE_CURVE(2,(#35648,#35649,#35650),.UNSPECIFIED.,.F.,.F.)
B_SPLINE_CURVE_WITH_KNOTS((3,3),(-0.27179589784536,-0.218746031477177),
 .UNSPECIFIED.)
CURVE()
GEOMETRIC_REPRESENTATION_ITEM()
RATIONAL_B_SPLINE_CURVE((1.02428162962094,1.02311336089455,1.02147610369988))
REPRESENTATION_ITEM('')
);
#528=(
BOUNDED_CURVE()
B_SPLINE_CURVE(2,(#35652,#35653,#35654),.UNSPECIFIED.,.F.,.F.)
B_SPLINE_CURVE_WITH_KNOTS((3,3),(-0.589144372850577,-0.536094506482401),
 .UNSPECIFIED.)
CURVE()
GEOMETRIC_REPRESENTATION_ITEM()
RATIONAL_B_SPLINE_CURVE((1.02147610369975,1.02311336089441,1.02428162962079))
REPRESENTATION_ITEM('')
);
#529=(
BOUNDED_CURVE()
B_SPLINE_CURVE(2,(#35658,#35659,#35660),.UNSPECIFIED.,.F.,.F.)
B_SPLINE_CURVE_WITH_KNOTS((3,3),(-0.271795897845361,-0.218746031477175),
 .UNSPECIFIED.)
CURVE()
GEOMETRIC_REPRESENTATION_ITEM()
RATIONAL_B_SPLINE_CURVE((1.02428162962098,1.02311336089459,1.02147610369992))
REPRESENTATION_ITEM('')
);
#530=(
BOUNDED_CURVE()
B_SPLINE_CURVE(2,(#35662,#35663,#35664),.UNSPECIFIED.,.F.,.F.)
B_SPLINE_CURVE_WITH_KNOTS((3,3),(-0.589144372850604,-0.536094506482412),
 .UNSPECIFIED.)
CURVE()
GEOMETRIC_REPRESENTATION_ITEM()
RATIONAL_B_SPLINE_CURVE((1.02147610370004,1.02311336089473,1.02428162962113))
REPRESENTATION_ITEM('')
);
#531=(
BOUNDED_CURVE()
B_SPLINE_CURVE(2,(#35668,#35669,#35670),.UNSPECIFIED.,.F.,.F.)
B_SPLINE_CURVE_WITH_KNOTS((3,3),(-0.271795897845358,-0.218746031477174),
 .UNSPECIFIED.)
CURVE()
GEOMETRIC_REPRESENTATION_ITEM()
RATIONAL_B_SPLINE_CURVE((1.02428162962094,1.02311336089455,1.02147610369988))
REPRESENTATION_ITEM('')
);
#532=(
BOUNDED_CURVE()
B_SPLINE_CURVE(2,(#35672,#35673,#35674),.UNSPECIFIED.,.F.,.F.)
B_SPLINE_CURVE_WITH_KNOTS((3,3),(-0.589144372850599,-0.536094506482411),
 .UNSPECIFIED.)
CURVE()
GEOMETRIC_REPRESENTATION_ITEM()
RATIONAL_B_SPLINE_CURVE((1.02147610369999,1.02311336089467,1.02428162962106))
REPRESENTATION_ITEM('')
);
#533=(
BOUNDED_CURVE()
B_SPLINE_CURVE(2,(#35678,#35679,#35680),.UNSPECIFIED.,.F.,.F.)
B_SPLINE_CURVE_WITH_KNOTS((3,3),(-0.271795897845357,-0.218746031477171),
 .UNSPECIFIED.)
CURVE()
GEOMETRIC_REPRESENTATION_ITEM()
RATIONAL_B_SPLINE_CURVE((1.02428162962099,1.0231133608946,1.02147610369993))
REPRESENTATION_ITEM('')
);
#534=(
BOUNDED_CURVE()
B_SPLINE_CURVE(2,(#35682,#35683,#35684),.UNSPECIFIED.,.F.,.F.)
B_SPLINE_CURVE_WITH_KNOTS((3,3),(-0.58914437285059,-0.536094506482401),
 .UNSPECIFIED.)
CURVE()
GEOMETRIC_REPRESENTATION_ITEM()
RATIONAL_B_SPLINE_CURVE((1.02147610369998,1.02311336089466,1.02428162962105))
REPRESENTATION_ITEM('')
);
#535=(
BOUNDED_CURVE()
B_SPLINE_CURVE(2,(#35688,#35689,#35690),.UNSPECIFIED.,.F.,.F.)
B_SPLINE_CURVE_WITH_KNOTS((3,3),(-0.271795897845351,-0.218746031477169),
 .UNSPECIFIED.)
CURVE()
GEOMETRIC_REPRESENTATION_ITEM()
RATIONAL_B_SPLINE_CURVE((1.02428162962091,1.02311336089453,1.02147610369986))
REPRESENTATION_ITEM('')
);
#536=(
BOUNDED_CURVE()
B_SPLINE_CURVE(2,(#35692,#35693,#35694),.UNSPECIFIED.,.F.,.F.)
B_SPLINE_CURVE_WITH_KNOTS((3,3),(-0.589144372850574,-0.536094506482395),
 .UNSPECIFIED.)
CURVE()
GEOMETRIC_REPRESENTATION_ITEM()
RATIONAL_B_SPLINE_CURVE((1.02147610369979,1.02311336089445,1.02428162962084))
REPRESENTATION_ITEM('')
);
#537=(
BOUNDED_CURVE()
B_SPLINE_CURVE(2,(#35698,#35699,#35700),.UNSPECIFIED.,.F.,.F.)
B_SPLINE_CURVE_WITH_KNOTS((3,3),(-0.271795897845357,-0.21874603147717),
 .UNSPECIFIED.)
CURVE()
GEOMETRIC_REPRESENTATION_ITEM()
RATIONAL_B_SPLINE_CURVE((1.02428162962101,1.02311336089462,1.02147610369994))
REPRESENTATION_ITEM('')
);
#538=(
BOUNDED_CURVE()
B_SPLINE_CURVE(2,(#35702,#35703,#35704),.UNSPECIFIED.,.F.,.F.)
B_SPLINE_CURVE_WITH_KNOTS((3,3),(-0.589144372850572,-0.536094506482391),
 .UNSPECIFIED.)
CURVE()
GEOMETRIC_REPRESENTATION_ITEM()
RATIONAL_B_SPLINE_CURVE((1.02147610369981,1.02311336089448,1.02428162962086))
REPRESENTATION_ITEM('')
);
#539=(
BOUNDED_CURVE()
B_SPLINE_CURVE(2,(#35708,#35709,#35710),.UNSPECIFIED.,.F.,.F.)
B_SPLINE_CURVE_WITH_KNOTS((3,3),(-0.271795897845355,-0.218746031477175),
 .UNSPECIFIED.)
CURVE()
GEOMETRIC_REPRESENTATION_ITEM()
RATIONAL_B_SPLINE_CURVE((1.02428162962088,1.02311336089449,1.02147610369983))
REPRESENTATION_ITEM('')
);
#540=(
BOUNDED_CURVE()
B_SPLINE_CURVE(2,(#35712,#35713,#35714),.UNSPECIFIED.,.F.,.F.)
B_SPLINE_CURVE_WITH_KNOTS((3,3),(-0.589144372850594,-0.53609450648241),
 .UNSPECIFIED.)
CURVE()
GEOMETRIC_REPRESENTATION_ITEM()
RATIONAL_B_SPLINE_CURVE((1.02147610369989,1.02311336089456,1.02428162962095))
REPRESENTATION_ITEM('')
);
#541=(
BOUNDED_CURVE()
B_SPLINE_CURVE(2,(#35718,#35719,#35720),.UNSPECIFIED.,.F.,.F.)
B_SPLINE_CURVE_WITH_KNOTS((3,3),(-0.271795897845355,-0.218746031477174),
 .UNSPECIFIED.)
CURVE()
GEOMETRIC_REPRESENTATION_ITEM()
RATIONAL_B_SPLINE_CURVE((1.0242816296209,1.02311336089451,1.02147610369984))
REPRESENTATION_ITEM('')
);
#542=(
BOUNDED_CURVE()
B_SPLINE_CURVE(2,(#35722,#35723,#35724),.UNSPECIFIED.,.F.,.F.)
B_SPLINE_CURVE_WITH_KNOTS((3,3),(-0.589144372850579,-0.536094506482395),
 .UNSPECIFIED.)
CURVE()
GEOMETRIC_REPRESENTATION_ITEM()
RATIONAL_B_SPLINE_CURVE((1.02147610369989,1.02311336089457,1.02428162962095))
REPRESENTATION_ITEM('')
);
#543=(
BOUNDED_CURVE()
B_SPLINE_CURVE(2,(#35728,#35729,#35730),.UNSPECIFIED.,.F.,.F.)
B_SPLINE_CURVE_WITH_KNOTS((3,3),(-0.271795897845349,-0.218746031477161),
 .UNSPECIFIED.)
CURVE()
GEOMETRIC_REPRESENTATION_ITEM()
RATIONAL_B_SPLINE_CURVE((1.02428162962106,1.02311336089467,1.02147610369999))
REPRESENTATION_ITEM('')
);
#544=(
BOUNDED_CURVE()
B_SPLINE_CURVE(2,(#35732,#35733,#35734),.UNSPECIFIED.,.F.,.F.)
B_SPLINE_CURVE_WITH_KNOTS((3,3),(-0.589144372850575,-0.536094506482389),
 .UNSPECIFIED.)
CURVE()
GEOMETRIC_REPRESENTATION_ITEM()
RATIONAL_B_SPLINE_CURVE((1.02147610369993,1.0231133608946,1.02428162962099))
REPRESENTATION_ITEM('')
);
#545=(
BOUNDED_CURVE()
B_SPLINE_CURVE(2,(#35738,#35739,#35740),.UNSPECIFIED.,.F.,.F.)
B_SPLINE_CURVE_WITH_KNOTS((3,3),(-0.271795897845358,-0.218746031477173),
 .UNSPECIFIED.)
CURVE()
GEOMETRIC_REPRESENTATION_ITEM()
RATIONAL_B_SPLINE_CURVE((1.02428162962099,1.0231133608946,1.02147610369993))
REPRESENTATION_ITEM('')
);
#546=(
BOUNDED_CURVE()
B_SPLINE_CURVE(2,(#35742,#35743,#35744),.UNSPECIFIED.,.F.,.F.)
B_SPLINE_CURVE_WITH_KNOTS((3,3),(-0.589144372850595,-0.536094506482406),
 .UNSPECIFIED.)
CURVE()
GEOMETRIC_REPRESENTATION_ITEM()
RATIONAL_B_SPLINE_CURVE((1.02147610369996,1.02311336089464,1.02428162962103))
REPRESENTATION_ITEM('')
);
#547=(
BOUNDED_CURVE()
B_SPLINE_CURVE(2,(#35748,#35749,#35750),.UNSPECIFIED.,.F.,.F.)
B_SPLINE_CURVE_WITH_KNOTS((3,3),(-0.271795897845368,-0.218746031477185),
 .UNSPECIFIED.)
CURVE()
GEOMETRIC_REPRESENTATION_ITEM()
RATIONAL_B_SPLINE_CURVE((1.02428162962092,1.02311336089454,1.02147610369987))
REPRESENTATION_ITEM('')
);
#548=(
BOUNDED_CURVE()
B_SPLINE_CURVE(2,(#35752,#35753,#35754),.UNSPECIFIED.,.F.,.F.)
B_SPLINE_CURVE_WITH_KNOTS((3,3),(-0.589144372850581,-0.536094506482396),
 .UNSPECIFIED.)
CURVE()
GEOMETRIC_REPRESENTATION_ITEM()
RATIONAL_B_SPLINE_CURVE((1.02147610369993,1.0231133608946,1.02428162962099))
REPRESENTATION_ITEM('')
);
#549=(
BOUNDED_CURVE()
B_SPLINE_CURVE(2,(#35758,#35759,#35760),.UNSPECIFIED.,.F.,.F.)
B_SPLINE_CURVE_WITH_KNOTS((3,3),(-0.271795897845348,-0.218746031477166),
 .UNSPECIFIED.)
CURVE()
GEOMETRIC_REPRESENTATION_ITEM()
RATIONAL_B_SPLINE_CURVE((1.02428162962094,1.02311336089455,1.02147610369988))
REPRESENTATION_ITEM('')
);
#550=(
BOUNDED_CURVE()
B_SPLINE_CURVE(2,(#35762,#35763,#35764),.UNSPECIFIED.,.F.,.F.)
B_SPLINE_CURVE_WITH_KNOTS((3,3),(-0.589144372850584,-0.536094506482403),
 .UNSPECIFIED.)
CURVE()
GEOMETRIC_REPRESENTATION_ITEM()
RATIONAL_B_SPLINE_CURVE((1.02147610369986,1.02311336089453,1.02428162962092))
REPRESENTATION_ITEM('')
);
#551=(
BOUNDED_CURVE()
B_SPLINE_CURVE(2,(#35767,#35768,#35769),.UNSPECIFIED.,.F.,.F.)
B_SPLINE_CURVE_WITH_KNOTS((3,3),(-0.271795897845352,-0.218746031477171),
 .UNSPECIFIED.)
CURVE()
GEOMETRIC_REPRESENTATION_ITEM()
RATIONAL_B_SPLINE_CURVE((1.02428162962091,1.02311336089452,1.02147610369985))
REPRESENTATION_ITEM('')
);
#552=(
BOUNDED_CURVE()
B_SPLINE_CURVE(2,(#36567,#36568,#36569),.UNSPECIFIED.,.F.,.F.)
B_SPLINE_CURVE_WITH_KNOTS((3,3),(0.536094506482412,0.5891443728506),
 .UNSPECIFIED.)
CURVE()
GEOMETRIC_REPRESENTATION_ITEM()
RATIONAL_B_SPLINE_CURVE((1.02428162962103,1.02311336089463,1.02147610369996))
REPRESENTATION_ITEM('')
);
#553=(
BOUNDED_CURVE()
B_SPLINE_CURVE(2,(#36573,#36574,#36575),.UNSPECIFIED.,.F.,.F.)
B_SPLINE_CURVE_WITH_KNOTS((3,3),(-0.27179589784535,-0.218746031477165),
 .UNSPECIFIED.)
CURVE()
GEOMETRIC_REPRESENTATION_ITEM()
RATIONAL_B_SPLINE_CURVE((1.02428162962098,1.02311336089459,1.02147610369991))
REPRESENTATION_ITEM('')
);
#554=(
BOUNDED_CURVE()
B_SPLINE_CURVE(2,(#36577,#36578,#36579),.UNSPECIFIED.,.F.,.F.)
B_SPLINE_CURVE_WITH_KNOTS((3,3),(-0.589144372850602,-0.536094506482414),
 .UNSPECIFIED.)
CURVE()
GEOMETRIC_REPRESENTATION_ITEM()
RATIONAL_B_SPLINE_CURVE((1.02147610369995,1.02311336089463,1.02428162962102))
REPRESENTATION_ITEM('')
);
#555=(
BOUNDED_CURVE()
B_SPLINE_CURVE(2,(#36583,#36584,#36585),.UNSPECIFIED.,.F.,.F.)
B_SPLINE_CURVE_WITH_KNOTS((3,3),(-0.271795897845356,-0.218746031477171),
 .UNSPECIFIED.)
CURVE()
GEOMETRIC_REPRESENTATION_ITEM()
RATIONAL_B_SPLINE_CURVE((1.02428162962098,1.02311336089459,1.02147610369991))
REPRESENTATION_ITEM('')
);
#556=(
BOUNDED_CURVE()
B_SPLINE_CURVE(2,(#36587,#36588,#36589),.UNSPECIFIED.,.F.,.F.)
B_SPLINE_CURVE_WITH_KNOTS((3,3),(-0.589144372850587,-0.536094506482402),
 .UNSPECIFIED.)
CURVE()
GEOMETRIC_REPRESENTATION_ITEM()
RATIONAL_B_SPLINE_CURVE((1.02147610369992,1.0231133608946,1.02428162962099))
REPRESENTATION_ITEM('')
);
#557=(
BOUNDED_CURVE()
B_SPLINE_CURVE(2,(#36593,#36594,#36595),.UNSPECIFIED.,.F.,.F.)
B_SPLINE_CURVE_WITH_KNOTS((3,3),(-0.271795897845345,-0.218746031477163),
 .UNSPECIFIED.)
CURVE()
GEOMETRIC_REPRESENTATION_ITEM()
RATIONAL_B_SPLINE_CURVE((1.02428162962094,1.02311336089455,1.02147610369988))
REPRESENTATION_ITEM('')
);
#558=(
BOUNDED_CURVE()
B_SPLINE_CURVE(2,(#36597,#36598,#36599),.UNSPECIFIED.,.F.,.F.)
B_SPLINE_CURVE_WITH_KNOTS((3,3),(-0.589144372850589,-0.536094506482405),
 .UNSPECIFIED.)
CURVE()
GEOMETRIC_REPRESENTATION_ITEM()
RATIONAL_B_SPLINE_CURVE((1.02147610369991,1.02311336089458,1.02428162962097))
REPRESENTATION_ITEM('')
);
#559=(
BOUNDED_CURVE()
B_SPLINE_CURVE(2,(#36603,#36604,#36605),.UNSPECIFIED.,.F.,.F.)
B_SPLINE_CURVE_WITH_KNOTS((3,3),(-0.271795897845365,-0.218746031477182),
 .UNSPECIFIED.)
CURVE()
GEOMETRIC_REPRESENTATION_ITEM()
RATIONAL_B_SPLINE_CURVE((1.02428162962089,1.02311336089451,1.02147610369984))
REPRESENTATION_ITEM('')
);
#560=(
BOUNDED_CURVE()
B_SPLINE_CURVE(2,(#36607,#36608,#36609),.UNSPECIFIED.,.F.,.F.)
B_SPLINE_CURVE_WITH_KNOTS((3,3),(-0.589144372850583,-0.536094506482398),
 .UNSPECIFIED.)
CURVE()
GEOMETRIC_REPRESENTATION_ITEM()
RATIONAL_B_SPLINE_CURVE((1.02147610369992,1.02311336089459,1.02428162962098))
REPRESENTATION_ITEM('')
);
#561=(
BOUNDED_CURVE()
B_SPLINE_CURVE(2,(#36613,#36614,#36615),.UNSPECIFIED.,.F.,.F.)
B_SPLINE_CURVE_WITH_KNOTS((3,3),(-0.271795897845351,-0.218746031477163),
 .UNSPECIFIED.)
CURVE()
GEOMETRIC_REPRESENTATION_ITEM()
RATIONAL_B_SPLINE_CURVE((1.02428162962104,1.02311336089465,1.02147610369997))
REPRESENTATION_ITEM('')
);
#562=(
BOUNDED_CURVE()
B_SPLINE_CURVE(2,(#36617,#36618,#36619),.UNSPECIFIED.,.F.,.F.)
B_SPLINE_CURVE_WITH_KNOTS((3,3),(-0.589144372850602,-0.536094506482419),
 .UNSPECIFIED.)
CURVE()
GEOMETRIC_REPRESENTATION_ITEM()
RATIONAL_B_SPLINE_CURVE((1.02147610369988,1.02311336089455,1.02428162962094))
REPRESENTATION_ITEM('')
);
#563=(
BOUNDED_CURVE()
B_SPLINE_CURVE(2,(#36623,#36624,#36625),.UNSPECIFIED.,.F.,.F.)
B_SPLINE_CURVE_WITH_KNOTS((3,3),(-0.271795897845357,-0.21874603147717),
 .UNSPECIFIED.)
CURVE()
GEOMETRIC_REPRESENTATION_ITEM()
RATIONAL_B_SPLINE_CURVE((1.02428162962102,1.02311336089463,1.02147610369995))
REPRESENTATION_ITEM('')
);
#564=(
BOUNDED_CURVE()
B_SPLINE_CURVE(2,(#36627,#36628,#36629),.UNSPECIFIED.,.F.,.F.)
B_SPLINE_CURVE_WITH_KNOTS((3,3),(-0.589144372850595,-0.536094506482411),
 .UNSPECIFIED.)
CURVE()
GEOMETRIC_REPRESENTATION_ITEM()
RATIONAL_B_SPLINE_CURVE((1.02147610369988,1.02311336089455,1.02428162962094))
REPRESENTATION_ITEM('')
);
#565=(
BOUNDED_CURVE()
B_SPLINE_CURVE(2,(#36633,#36634,#36635),.UNSPECIFIED.,.F.,.F.)
B_SPLINE_CURVE_WITH_KNOTS((3,3),(-0.271795897845351,-0.218746031477165),
 .UNSPECIFIED.)
CURVE()
GEOMETRIC_REPRESENTATION_ITEM()
RATIONAL_B_SPLINE_CURVE((1.02428162962101,1.02311336089462,1.02147610369994))
REPRESENTATION_ITEM('')
);
#566=(
BOUNDED_CURVE()
B_SPLINE_CURVE(2,(#36637,#36638,#36639),.UNSPECIFIED.,.F.,.F.)
B_SPLINE_CURVE_WITH_KNOTS((3,3),(-0.589144372850605,-0.536094506482423),
 .UNSPECIFIED.)
CURVE()
GEOMETRIC_REPRESENTATION_ITEM()
RATIONAL_B_SPLINE_CURVE((1.02147610369987,1.02311336089453,1.02428162962092))
REPRESENTATION_ITEM('')
);
#567=(
BOUNDED_CURVE()
B_SPLINE_CURVE(2,(#36643,#36644,#36645),.UNSPECIFIED.,.F.,.F.)
B_SPLINE_CURVE_WITH_KNOTS((3,3),(-0.271795897845359,-0.218746031477179),
 .UNSPECIFIED.)
CURVE()
GEOMETRIC_REPRESENTATION_ITEM()
RATIONAL_B_SPLINE_CURVE((1.02428162962085,1.02311336089447,1.02147610369981))
REPRESENTATION_ITEM('')
);
#568=(
BOUNDED_CURVE()
B_SPLINE_CURVE(2,(#36647,#36648,#36649),.UNSPECIFIED.,.F.,.F.)
B_SPLINE_CURVE_WITH_KNOTS((3,3),(-0.589144372850621,-0.536094506482433),
 .UNSPECIFIED.)
CURVE()
GEOMETRIC_REPRESENTATION_ITEM()
RATIONAL_B_SPLINE_CURVE((1.02147610369998,1.02311336089466,1.02428162962105))
REPRESENTATION_ITEM('')
);
#569=(
BOUNDED_CURVE()
B_SPLINE_CURVE(2,(#36653,#36654,#36655),.UNSPECIFIED.,.F.,.F.)
B_SPLINE_CURVE_WITH_KNOTS((3,3),(-0.271795897845357,-0.218746031477166),
 .UNSPECIFIED.)
CURVE()
GEOMETRIC_REPRESENTATION_ITEM()
RATIONAL_B_SPLINE_CURVE((1.02428162962107,1.02311336089468,1.0214761037))
REPRESENTATION_ITEM('')
);
#570=(
BOUNDED_CURVE()
B_SPLINE_CURVE(2,(#36657,#36658,#36659),.UNSPECIFIED.,.F.,.F.)
B_SPLINE_CURVE_WITH_KNOTS((3,3),(-0.589144372850594,-0.536094506482414),
 .UNSPECIFIED.)
CURVE()
GEOMETRIC_REPRESENTATION_ITEM()
RATIONAL_B_SPLINE_CURVE((1.02147610369981,1.02311336089447,1.02428162962085))
REPRESENTATION_ITEM('')
);
#571=(
BOUNDED_CURVE()
B_SPLINE_CURVE(2,(#36663,#36664,#36665),.UNSPECIFIED.,.F.,.F.)
B_SPLINE_CURVE_WITH_KNOTS((3,3),(-0.271795897845359,-0.218746031477176),
 .UNSPECIFIED.)
CURVE()
GEOMETRIC_REPRESENTATION_ITEM()
RATIONAL_B_SPLINE_CURVE((1.02428162962093,1.02311336089454,1.02147610369987))
REPRESENTATION_ITEM('')
);
#572=(
BOUNDED_CURVE()
B_SPLINE_CURVE(2,(#36667,#36668,#36669),.UNSPECIFIED.,.F.,.F.)
B_SPLINE_CURVE_WITH_KNOTS((3,3),(-0.589144372850597,-0.536094506482409),
 .UNSPECIFIED.)
CURVE()
GEOMETRIC_REPRESENTATION_ITEM()
RATIONAL_B_SPLINE_CURVE((1.02147610369995,1.02311336089463,1.02428162962102))
REPRESENTATION_ITEM('')
);
#573=(
BOUNDED_CURVE()
B_SPLINE_CURVE(2,(#36673,#36674,#36675),.UNSPECIFIED.,.F.,.F.)
B_SPLINE_CURVE_WITH_KNOTS((3,3),(-0.271795897845349,-0.218746031477168),
 .UNSPECIFIED.)
CURVE()
GEOMETRIC_REPRESENTATION_ITEM()
RATIONAL_B_SPLINE_CURVE((1.02428162962088,1.0231133608945,1.02147610369983))
REPRESENTATION_ITEM('')
);
#574=(
BOUNDED_CURVE()
B_SPLINE_CURVE(2,(#36677,#36678,#36679),.UNSPECIFIED.,.F.,.F.)
B_SPLINE_CURVE_WITH_KNOTS((3,3),(-0.589144372850612,-0.536094506482427),
 .UNSPECIFIED.)
CURVE()
GEOMETRIC_REPRESENTATION_ITEM()
RATIONAL_B_SPLINE_CURVE((1.02147610369991,1.02311336089458,1.02428162962097))
REPRESENTATION_ITEM('')
);
#575=(
BOUNDED_CURVE()
B_SPLINE_CURVE(2,(#36683,#36684,#36685),.UNSPECIFIED.,.F.,.F.)
B_SPLINE_CURVE_WITH_KNOTS((3,3),(-0.27179589784536,-0.218746031477173),
 .UNSPECIFIED.)
CURVE()
GEOMETRIC_REPRESENTATION_ITEM()
RATIONAL_B_SPLINE_CURVE((1.02428162962101,1.02311336089462,1.02147610369994))
REPRESENTATION_ITEM('')
);
#576=(
BOUNDED_CURVE()
B_SPLINE_CURVE(2,(#36687,#36688,#36689),.UNSPECIFIED.,.F.,.F.)
B_SPLINE_CURVE_WITH_KNOTS((3,3),(-0.589144372850594,-0.536094506482412),
 .UNSPECIFIED.)
CURVE()
GEOMETRIC_REPRESENTATION_ITEM()
RATIONAL_B_SPLINE_CURVE((1.02147610369986,1.02311336089453,1.02428162962092))
REPRESENTATION_ITEM('')
);
#577=(
BOUNDED_CURVE()
B_SPLINE_CURVE(2,(#36693,#36694,#36695),.UNSPECIFIED.,.F.,.F.)
B_SPLINE_CURVE_WITH_KNOTS((3,3),(-0.271795897845352,-0.218746031477168),
 .UNSPECIFIED.)
CURVE()
GEOMETRIC_REPRESENTATION_ITEM()
RATIONAL_B_SPLINE_CURVE((1.02428162962095,1.02311336089456,1.02147610369989))
REPRESENTATION_ITEM('')
);
#578=(
BOUNDED_CURVE()
B_SPLINE_CURVE(2,(#36697,#36698,#36699),.UNSPECIFIED.,.F.,.F.)
B_SPLINE_CURVE_WITH_KNOTS((3,3),(-0.589144372850596,-0.536094506482406),
 .UNSPECIFIED.)
CURVE()
GEOMETRIC_REPRESENTATION_ITEM()
RATIONAL_B_SPLINE_CURVE((1.02147610369999,1.02311336089467,1.02428162962107))
REPRESENTATION_ITEM('')
);
#579=(
BOUNDED_CURVE()
B_SPLINE_CURVE(2,(#36703,#36704,#36705),.UNSPECIFIED.,.F.,.F.)
B_SPLINE_CURVE_WITH_KNOTS((3,3),(-0.271795897845352,-0.218746031477168),
 .UNSPECIFIED.)
CURVE()
GEOMETRIC_REPRESENTATION_ITEM()
RATIONAL_B_SPLINE_CURVE((1.02428162962096,1.02311336089457,1.0214761036999))
REPRESENTATION_ITEM('')
);
#580=(
BOUNDED_CURVE()
B_SPLINE_CURVE(2,(#36707,#36708,#36709),.UNSPECIFIED.,.F.,.F.)
B_SPLINE_CURVE_WITH_KNOTS((3,3),(-0.589144372850588,-0.536094506482405),
 .UNSPECIFIED.)
CURVE()
GEOMETRIC_REPRESENTATION_ITEM()
RATIONAL_B_SPLINE_CURVE((1.02147610369987,1.02311336089454,1.02428162962093))
REPRESENTATION_ITEM('')
);
#581=(
BOUNDED_CURVE()
B_SPLINE_CURVE(2,(#36713,#36714,#36715),.UNSPECIFIED.,.F.,.F.)
B_SPLINE_CURVE_WITH_KNOTS((3,3),(-0.271795897845354,-0.218746031477172),
 .UNSPECIFIED.)
CURVE()
GEOMETRIC_REPRESENTATION_ITEM()
RATIONAL_B_SPLINE_CURVE((1.0242816296209,1.02311336089451,1.02147610369984))
REPRESENTATION_ITEM('')
);
#582=(
BOUNDED_CURVE()
B_SPLINE_CURVE(2,(#36717,#36718,#36719),.UNSPECIFIED.,.F.,.F.)
B_SPLINE_CURVE_WITH_KNOTS((3,3),(-0.589144372850593,-0.536094506482412),
 .UNSPECIFIED.)
CURVE()
GEOMETRIC_REPRESENTATION_ITEM()
RATIONAL_B_SPLINE_CURVE((1.02147610369985,1.02311336089452,1.0242816296209))
REPRESENTATION_ITEM('')
);
#583=(
BOUNDED_CURVE()
B_SPLINE_CURVE(2,(#36723,#36724,#36725),.UNSPECIFIED.,.F.,.F.)
B_SPLINE_CURVE_WITH_KNOTS((3,3),(-0.271795897845351,-0.218746031477167),
 .UNSPECIFIED.)
CURVE()
GEOMETRIC_REPRESENTATION_ITEM()
RATIONAL_B_SPLINE_CURVE((1.02428162962095,1.02311336089456,1.02147610369989))
REPRESENTATION_ITEM('')
);
#584=(
BOUNDED_CURVE()
B_SPLINE_CURVE(2,(#36727,#36728,#36729),.UNSPECIFIED.,.F.,.F.)
B_SPLINE_CURVE_WITH_KNOTS((3,3),(-0.589144372850603,-0.536094506482421),
 .UNSPECIFIED.)
CURVE()
GEOMETRIC_REPRESENTATION_ITEM()
RATIONAL_B_SPLINE_CURVE((1.02147610369987,1.02311336089454,1.02428162962092))
REPRESENTATION_ITEM('')
);
#585=(
BOUNDED_CURVE()
B_SPLINE_CURVE(2,(#36733,#36734,#36735),.UNSPECIFIED.,.F.,.F.)
B_SPLINE_CURVE_WITH_KNOTS((3,3),(-0.271795897845345,-0.218746031477162),
 .UNSPECIFIED.)
CURVE()
GEOMETRIC_REPRESENTATION_ITEM()
RATIONAL_B_SPLINE_CURVE((1.02428162962095,1.02311336089456,1.02147610369989))
REPRESENTATION_ITEM('')
);
#586=(
BOUNDED_CURVE()
B_SPLINE_CURVE(2,(#36737,#36738,#36739),.UNSPECIFIED.,.F.,.F.)
B_SPLINE_CURVE_WITH_KNOTS((3,3),(-0.589144372850587,-0.536094506482405),
 .UNSPECIFIED.)
CURVE()
GEOMETRIC_REPRESENTATION_ITEM()
RATIONAL_B_SPLINE_CURVE((1.02147610369987,1.02311336089454,1.02428162962092))
REPRESENTATION_ITEM('')
);
#587=(
BOUNDED_CURVE()
B_SPLINE_CURVE(2,(#36743,#36744,#36745),.UNSPECIFIED.,.F.,.F.)
B_SPLINE_CURVE_WITH_KNOTS((3,3),(-0.271795897845357,-0.218746031477178),
 .UNSPECIFIED.)
CURVE()
GEOMETRIC_REPRESENTATION_ITEM()
RATIONAL_B_SPLINE_CURVE((1.02428162962083,1.02311336089445,1.02147610369978))
REPRESENTATION_ITEM('')
);
#588=(
BOUNDED_CURVE()
B_SPLINE_CURVE(2,(#36747,#36748,#36749),.UNSPECIFIED.,.F.,.F.)
B_SPLINE_CURVE_WITH_KNOTS((3,3),(-0.589144372850587,-0.536094506482403),
 .UNSPECIFIED.)
CURVE()
GEOMETRIC_REPRESENTATION_ITEM()
RATIONAL_B_SPLINE_CURVE((1.02147610369989,1.02311336089456,1.02428162962095))
REPRESENTATION_ITEM('')
);
#589=(
BOUNDED_CURVE()
B_SPLINE_CURVE(2,(#36753,#36754,#36755),.UNSPECIFIED.,.F.,.F.)
B_SPLINE_CURVE_WITH_KNOTS((3,3),(-0.271795897845361,-0.218746031477177),
 .UNSPECIFIED.)
CURVE()
GEOMETRIC_REPRESENTATION_ITEM()
RATIONAL_B_SPLINE_CURVE((1.02428162962093,1.02311336089454,1.02147610369987))
REPRESENTATION_ITEM('')
);
#590=(
BOUNDED_CURVE()
B_SPLINE_CURVE(2,(#36757,#36758,#36759),.UNSPECIFIED.,.F.,.F.)
B_SPLINE_CURVE_WITH_KNOTS((3,3),(-0.589144372850603,-0.536094506482419),
 .UNSPECIFIED.)
CURVE()
GEOMETRIC_REPRESENTATION_ITEM()
RATIONAL_B_SPLINE_CURVE((1.02147610369989,1.02311336089457,1.02428162962095))
REPRESENTATION_ITEM('')
);
#591=(
BOUNDED_CURVE()
B_SPLINE_CURVE(2,(#36763,#36764,#36765),.UNSPECIFIED.,.F.,.F.)
B_SPLINE_CURVE_WITH_KNOTS((3,3),(-0.271795897845354,-0.21874603147717),
 .UNSPECIFIED.)
CURVE()
GEOMETRIC_REPRESENTATION_ITEM()
RATIONAL_B_SPLINE_CURVE((1.02428162962096,1.02311336089457,1.0214761036999))
REPRESENTATION_ITEM('')
);
#592=(
BOUNDED_CURVE()
B_SPLINE_CURVE(2,(#36767,#36768,#36769),.UNSPECIFIED.,.F.,.F.)
B_SPLINE_CURVE_WITH_KNOTS((3,3),(-0.589144372850597,-0.536094506482414),
 .UNSPECIFIED.)
CURVE()
GEOMETRIC_REPRESENTATION_ITEM()
RATIONAL_B_SPLINE_CURVE((1.02147610369986,1.02311336089453,1.02428162962092))
REPRESENTATION_ITEM('')
);
#593=(
BOUNDED_CURVE()
B_SPLINE_CURVE(2,(#36773,#36774,#36775),.UNSPECIFIED.,.F.,.F.)
B_SPLINE_CURVE_WITH_KNOTS((3,3),(-0.271795897845355,-0.218746031477174),
 .UNSPECIFIED.)
CURVE()
GEOMETRIC_REPRESENTATION_ITEM()
RATIONAL_B_SPLINE_CURVE((1.02428162962089,1.0231133608945,1.02147610369983))
REPRESENTATION_ITEM('')
);
#594=(
BOUNDED_CURVE()
B_SPLINE_CURVE(2,(#36777,#36778,#36779),.UNSPECIFIED.,.F.,.F.)
B_SPLINE_CURVE_WITH_KNOTS((3,3),(-0.589144372850588,-0.536094506482404),
 .UNSPECIFIED.)
CURVE()
GEOMETRIC_REPRESENTATION_ITEM()
RATIONAL_B_SPLINE_CURVE((1.02147610369988,1.02311336089455,1.02428162962094))
REPRESENTATION_ITEM('')
);
#595=(
BOUNDED_CURVE()
B_SPLINE_CURVE(2,(#36783,#36784,#36785),.UNSPECIFIED.,.F.,.F.)
B_SPLINE_CURVE_WITH_KNOTS((3,3),(-0.271795897845348,-0.218746031477163),
 .UNSPECIFIED.)
CURVE()
GEOMETRIC_REPRESENTATION_ITEM()
RATIONAL_B_SPLINE_CURVE((1.02428162962099,1.0231133608946,1.02147610369993))
REPRESENTATION_ITEM('')
);
#596=(
BOUNDED_CURVE()
B_SPLINE_CURVE(2,(#36787,#36788,#36789),.UNSPECIFIED.,.F.,.F.)
B_SPLINE_CURVE_WITH_KNOTS((3,3),(-0.589144372850592,-0.536094506482408),
 .UNSPECIFIED.)
CURVE()
GEOMETRIC_REPRESENTATION_ITEM()
RATIONAL_B_SPLINE_CURVE((1.0214761036999,1.02311336089457,1.02428162962096))
REPRESENTATION_ITEM('')
);
#597=(
BOUNDED_CURVE()
B_SPLINE_CURVE(2,(#36793,#36794,#36795),.UNSPECIFIED.,.F.,.F.)
B_SPLINE_CURVE_WITH_KNOTS((3,3),(-0.271795897845357,-0.218746031477176),
 .UNSPECIFIED.)
CURVE()
GEOMETRIC_REPRESENTATION_ITEM()
RATIONAL_B_SPLINE_CURVE((1.02428162962088,1.02311336089449,1.02147610369983))
REPRESENTATION_ITEM('')
);
#598=(
BOUNDED_CURVE()
B_SPLINE_CURVE(2,(#36797,#36798,#36799),.UNSPECIFIED.,.F.,.F.)
B_SPLINE_CURVE_WITH_KNOTS((3,3),(-0.589144372850592,-0.536094506482406),
 .UNSPECIFIED.)
CURVE()
GEOMETRIC_REPRESENTATION_ITEM()
RATIONAL_B_SPLINE_CURVE((1.02147610369992,1.02311336089459,1.02428162962098))
REPRESENTATION_ITEM('')
);
#599=(
BOUNDED_CURVE()
B_SPLINE_CURVE(2,(#36803,#36804,#36805),.UNSPECIFIED.,.F.,.F.)
B_SPLINE_CURVE_WITH_KNOTS((3,3),(-0.27179589784536,-0.218746031477179),
 .UNSPECIFIED.)
CURVE()
GEOMETRIC_REPRESENTATION_ITEM()
RATIONAL_B_SPLINE_CURVE((1.02428162962089,1.0231133608945,1.02147610369984))
REPRESENTATION_ITEM('')
);
#600=(
BOUNDED_CURVE()
B_SPLINE_CURVE(2,(#36807,#36808,#36809),.UNSPECIFIED.,.F.,.F.)
B_SPLINE_CURVE_WITH_KNOTS((3,3),(-0.589144372850584,-0.536094506482402),
 .UNSPECIFIED.)
CURVE()
GEOMETRIC_REPRESENTATION_ITEM()
RATIONAL_B_SPLINE_CURVE((1.02147610369986,1.02311336089453,1.02428162962092))
REPRESENTATION_ITEM('')
);
#601=(
BOUNDED_CURVE()
B_SPLINE_CURVE(2,(#36813,#36814,#36815),.UNSPECIFIED.,.F.,.F.)
B_SPLINE_CURVE_WITH_KNOTS((3,3),(-0.271795897845342,-0.218746031477156),
 .UNSPECIFIED.)
CURVE()
GEOMETRIC_REPRESENTATION_ITEM()
RATIONAL_B_SPLINE_CURVE((1.02428162962101,1.02311336089462,1.02147610369994))
REPRESENTATION_ITEM('')
);
#602=(
BOUNDED_CURVE()
B_SPLINE_CURVE(2,(#36817,#36818,#36819),.UNSPECIFIED.,.F.,.F.)
B_SPLINE_CURVE_WITH_KNOTS((3,3),(-0.589144372850578,-0.536094506482394),
 .UNSPECIFIED.)
CURVE()
GEOMETRIC_REPRESENTATION_ITEM()
RATIONAL_B_SPLINE_CURVE((1.02147610369987,1.02311336089454,1.02428162962093))
REPRESENTATION_ITEM('')
);
#603=(
BOUNDED_CURVE()
B_SPLINE_CURVE(2,(#36823,#36824,#36825),.UNSPECIFIED.,.F.,.F.)
B_SPLINE_CURVE_WITH_KNOTS((3,3),(-0.271795897845354,-0.21874603147717),
 .UNSPECIFIED.)
CURVE()
GEOMETRIC_REPRESENTATION_ITEM()
RATIONAL_B_SPLINE_CURVE((1.02428162962094,1.02311336089455,1.02147610369988))
REPRESENTATION_ITEM('')
);
#604=(
BOUNDED_CURVE()
B_SPLINE_CURVE(2,(#36827,#36828,#36829),.UNSPECIFIED.,.F.,.F.)
B_SPLINE_CURVE_WITH_KNOTS((3,3),(-0.589144372850586,-0.536094506482403),
 .UNSPECIFIED.)
CURVE()
GEOMETRIC_REPRESENTATION_ITEM()
RATIONAL_B_SPLINE_CURVE((1.02147610369988,1.02311336089455,1.02428162962094))
REPRESENTATION_ITEM('')
);
#605=(
BOUNDED_CURVE()
B_SPLINE_CURVE(2,(#36833,#36834,#36835),.UNSPECIFIED.,.F.,.F.)
B_SPLINE_CURVE_WITH_KNOTS((3,3),(-0.271795897845349,-0.218746031477164),
 .UNSPECIFIED.)
CURVE()
GEOMETRIC_REPRESENTATION_ITEM()
RATIONAL_B_SPLINE_CURVE((1.02428162962096,1.02311336089458,1.0214761036999))
REPRESENTATION_ITEM('')
);
#606=(
BOUNDED_CURVE()
B_SPLINE_CURVE(2,(#36837,#36838,#36839),.UNSPECIFIED.,.F.,.F.)
B_SPLINE_CURVE_WITH_KNOTS((3,3),(-0.589144372850588,-0.536094506482402),
 .UNSPECIFIED.)
CURVE()
GEOMETRIC_REPRESENTATION_ITEM()
RATIONAL_B_SPLINE_CURVE((1.02147610369991,1.02311336089459,1.02428162962098))
REPRESENTATION_ITEM('')
);
#607=(
BOUNDED_CURVE()
B_SPLINE_CURVE(2,(#36843,#36844,#36845),.UNSPECIFIED.,.F.,.F.)
B_SPLINE_CURVE_WITH_KNOTS((3,3),(-0.271795897845353,-0.218746031477165),
 .UNSPECIFIED.)
CURVE()
GEOMETRIC_REPRESENTATION_ITEM()
RATIONAL_B_SPLINE_CURVE((1.02428162962104,1.02311336089465,1.02147610369997))
REPRESENTATION_ITEM('')
);
#608=(
BOUNDED_CURVE()
B_SPLINE_CURVE(2,(#36847,#36848,#36849),.UNSPECIFIED.,.F.,.F.)
B_SPLINE_CURVE_WITH_KNOTS((3,3),(-0.589144372850592,-0.536094506482409),
 .UNSPECIFIED.)
CURVE()
GEOMETRIC_REPRESENTATION_ITEM()
RATIONAL_B_SPLINE_CURVE((1.02147610369986,1.02311336089453,1.02428162962092))
REPRESENTATION_ITEM('')
);
#609=(
BOUNDED_CURVE()
B_SPLINE_CURVE(2,(#36853,#36854,#36855),.UNSPECIFIED.,.F.,.F.)
B_SPLINE_CURVE_WITH_KNOTS((3,3),(-0.271795897845343,-0.218746031477159),
 .UNSPECIFIED.)
CURVE()
GEOMETRIC_REPRESENTATION_ITEM()
RATIONAL_B_SPLINE_CURVE((1.02428162962097,1.02311336089458,1.0214761036999))
REPRESENTATION_ITEM('')
);
#610=(
BOUNDED_CURVE()
B_SPLINE_CURVE(2,(#36857,#36858,#36859),.UNSPECIFIED.,.F.,.F.)
B_SPLINE_CURVE_WITH_KNOTS((3,3),(-0.589144372850575,-0.536094506482395),
 .UNSPECIFIED.)
CURVE()
GEOMETRIC_REPRESENTATION_ITEM()
RATIONAL_B_SPLINE_CURVE((1.0214761036998,1.02311336089446,1.02428162962085))
REPRESENTATION_ITEM('')
);
#611=(
BOUNDED_CURVE()
B_SPLINE_CURVE(2,(#36863,#36864,#36865),.UNSPECIFIED.,.F.,.F.)
B_SPLINE_CURVE_WITH_KNOTS((3,3),(-0.271795897845356,-0.218746031477172),
 .UNSPECIFIED.)
CURVE()
GEOMETRIC_REPRESENTATION_ITEM()
RATIONAL_B_SPLINE_CURVE((1.02428162962094,1.02311336089456,1.02147610369988))
REPRESENTATION_ITEM('')
);
#612=(
BOUNDED_CURVE()
B_SPLINE_CURVE(2,(#36867,#36868,#36869),.UNSPECIFIED.,.F.,.F.)
B_SPLINE_CURVE_WITH_KNOTS((3,3),(-0.589144372850588,-0.536094506482404),
 .UNSPECIFIED.)
CURVE()
GEOMETRIC_REPRESENTATION_ITEM()
RATIONAL_B_SPLINE_CURVE((1.02147610369989,1.02311336089456,1.02428162962095))
REPRESENTATION_ITEM('')
);
#613=(
BOUNDED_CURVE()
B_SPLINE_CURVE(2,(#36873,#36874,#36875),.UNSPECIFIED.,.F.,.F.)
B_SPLINE_CURVE_WITH_KNOTS((3,3),(-0.271795897845355,-0.21874603147717),
 .UNSPECIFIED.)
CURVE()
GEOMETRIC_REPRESENTATION_ITEM()
RATIONAL_B_SPLINE_CURVE((1.02428162962098,1.02311336089459,1.02147610369992))
REPRESENTATION_ITEM('')
);
#614=(
BOUNDED_CURVE()
B_SPLINE_CURVE(2,(#36877,#36878,#36879),.UNSPECIFIED.,.F.,.F.)
B_SPLINE_CURVE_WITH_KNOTS((3,3),(-0.589144372850597,-0.536094506482411),
 .UNSPECIFIED.)
CURVE()
GEOMETRIC_REPRESENTATION_ITEM()
RATIONAL_B_SPLINE_CURVE((1.02147610369993,1.0231133608946,1.024281629621))
REPRESENTATION_ITEM('')
);
#615=(
BOUNDED_CURVE()
B_SPLINE_CURVE(2,(#36883,#36884,#36885),.UNSPECIFIED.,.F.,.F.)
B_SPLINE_CURVE_WITH_KNOTS((3,3),(-0.271795897845346,-0.218746031477162),
 .UNSPECIFIED.)
CURVE()
GEOMETRIC_REPRESENTATION_ITEM()
RATIONAL_B_SPLINE_CURVE((1.02428162962096,1.02311336089457,1.0214761036999))
REPRESENTATION_ITEM('')
);
#616=(
BOUNDED_CURVE()
B_SPLINE_CURVE(2,(#36887,#36888,#36889),.UNSPECIFIED.,.F.,.F.)
B_SPLINE_CURVE_WITH_KNOTS((3,3),(-0.589144372850587,-0.536094506482401),
 .UNSPECIFIED.)
CURVE()
GEOMETRIC_REPRESENTATION_ITEM()
RATIONAL_B_SPLINE_CURVE((1.02147610369994,1.02311336089461,1.024281629621))
REPRESENTATION_ITEM('')
);
#617=(
BOUNDED_CURVE()
B_SPLINE_CURVE(2,(#36893,#36894,#36895),.UNSPECIFIED.,.F.,.F.)
B_SPLINE_CURVE_WITH_KNOTS((3,3),(-0.271795897845345,-0.218746031477163),
 .UNSPECIFIED.)
CURVE()
GEOMETRIC_REPRESENTATION_ITEM()
RATIONAL_B_SPLINE_CURVE((1.02428162962093,1.02311336089454,1.02147610369987))
REPRESENTATION_ITEM('')
);
#618=(
BOUNDED_CURVE()
B_SPLINE_CURVE(2,(#36897,#36898,#36899),.UNSPECIFIED.,.F.,.F.)
B_SPLINE_CURVE_WITH_KNOTS((3,3),(-0.589144372850582,-0.5360945064824),
 .UNSPECIFIED.)
CURVE()
GEOMETRIC_REPRESENTATION_ITEM()
RATIONAL_B_SPLINE_CURVE((1.02147610369986,1.02311336089452,1.02428162962091))
REPRESENTATION_ITEM('')
);
#619=(
BOUNDED_CURVE()
B_SPLINE_CURVE(2,(#36903,#36904,#36905),.UNSPECIFIED.,.F.,.F.)
B_SPLINE_CURVE_WITH_KNOTS((3,3),(-0.271795897845348,-0.218746031477163),
 .UNSPECIFIED.)
CURVE()
GEOMETRIC_REPRESENTATION_ITEM()
RATIONAL_B_SPLINE_CURVE((1.02428162962098,1.02311336089459,1.02147610369992))
REPRESENTATION_ITEM('')
);
#620=(
BOUNDED_CURVE()
B_SPLINE_CURVE(2,(#36907,#36908,#36909),.UNSPECIFIED.,.F.,.F.)
B_SPLINE_CURVE_WITH_KNOTS((3,3),(-0.589144372850595,-0.536094506482406),
 .UNSPECIFIED.)
CURVE()
GEOMETRIC_REPRESENTATION_ITEM()
RATIONAL_B_SPLINE_CURVE((1.02147610369997,1.02311336089465,1.02428162962104))
REPRESENTATION_ITEM('')
);
#621=(
BOUNDED_CURVE()
B_SPLINE_CURVE(2,(#36913,#36914,#36915),.UNSPECIFIED.,.F.,.F.)
B_SPLINE_CURVE_WITH_KNOTS((3,3),(-0.271795897845349,-0.218746031477164),
 .UNSPECIFIED.)
CURVE()
GEOMETRIC_REPRESENTATION_ITEM()
RATIONAL_B_SPLINE_CURVE((1.02428162962097,1.02311336089458,1.02147610369991))
REPRESENTATION_ITEM('')
);
#622=(
BOUNDED_CURVE()
B_SPLINE_CURVE(2,(#36917,#36918,#36919),.UNSPECIFIED.,.F.,.F.)
B_SPLINE_CURVE_WITH_KNOTS((3,3),(-0.589144372850605,-0.536094506482415),
 .UNSPECIFIED.)
CURVE()
GEOMETRIC_REPRESENTATION_ITEM()
RATIONAL_B_SPLINE_CURVE((1.02147610369999,1.02311336089467,1.02428162962106))
REPRESENTATION_ITEM('')
);
#623=(
BOUNDED_CURVE()
B_SPLINE_CURVE(2,(#36923,#36924,#36925),.UNSPECIFIED.,.F.,.F.)
B_SPLINE_CURVE_WITH_KNOTS((3,3),(-0.271795897845347,-0.218746031477163),
 .UNSPECIFIED.)
CURVE()
GEOMETRIC_REPRESENTATION_ITEM()
RATIONAL_B_SPLINE_CURVE((1.02428162962095,1.02311336089456,1.02147610369989))
REPRESENTATION_ITEM('')
);
#624=(
BOUNDED_CURVE()
B_SPLINE_CURVE(2,(#36927,#36928,#36929),.UNSPECIFIED.,.F.,.F.)
B_SPLINE_CURVE_WITH_KNOTS((3,3),(-0.589144372850588,-0.53609450648241),
 .UNSPECIFIED.)
CURVE()
GEOMETRIC_REPRESENTATION_ITEM()
RATIONAL_B_SPLINE_CURVE((1.0214761036998,1.02311336089446,1.02428162962085))
REPRESENTATION_ITEM('')
);
#625=(
BOUNDED_CURVE()
B_SPLINE_CURVE(2,(#36933,#36934,#36935),.UNSPECIFIED.,.F.,.F.)
B_SPLINE_CURVE_WITH_KNOTS((3,3),(-0.271795897845344,-0.218746031477158),
 .UNSPECIFIED.)
CURVE()
GEOMETRIC_REPRESENTATION_ITEM()
RATIONAL_B_SPLINE_CURVE((1.024281629621,1.02311336089461,1.02147610369994))
REPRESENTATION_ITEM('')
);
#626=(
BOUNDED_CURVE()
B_SPLINE_CURVE(2,(#36937,#36938,#36939),.UNSPECIFIED.,.F.,.F.)
B_SPLINE_CURVE_WITH_KNOTS((3,3),(-0.589144372850618,-0.536094506482433),
 .UNSPECIFIED.)
CURVE()
GEOMETRIC_REPRESENTATION_ITEM()
RATIONAL_B_SPLINE_CURVE((1.0214761036999,1.02311336089457,1.02428162962096))
REPRESENTATION_ITEM('')
);
#627=(
BOUNDED_CURVE()
B_SPLINE_CURVE(2,(#36943,#36944,#36945),.UNSPECIFIED.,.F.,.F.)
B_SPLINE_CURVE_WITH_KNOTS((3,3),(-0.271795897845356,-0.218746031477172),
 .UNSPECIFIED.)
CURVE()
GEOMETRIC_REPRESENTATION_ITEM()
RATIONAL_B_SPLINE_CURVE((1.02428162962095,1.02311336089456,1.02147610369989))
REPRESENTATION_ITEM('')
);
#628=(
BOUNDED_CURVE()
B_SPLINE_CURVE(2,(#36947,#36948,#36949),.UNSPECIFIED.,.F.,.F.)
B_SPLINE_CURVE_WITH_KNOTS((3,3),(-0.589144372850593,-0.53609450648241),
 .UNSPECIFIED.)
CURVE()
GEOMETRIC_REPRESENTATION_ITEM()
RATIONAL_B_SPLINE_CURVE((1.02147610369989,1.02311336089456,1.02428162962095))
REPRESENTATION_ITEM('')
);
#629=(
BOUNDED_CURVE()
B_SPLINE_CURVE(2,(#36953,#36954,#36955),.UNSPECIFIED.,.F.,.F.)
B_SPLINE_CURVE_WITH_KNOTS((3,3),(-0.271795897845356,-0.27009889353462),
 .UNSPECIFIED.)
CURVE()
GEOMETRIC_REPRESENTATION_ITEM()
RATIONAL_B_SPLINE_CURVE((1.024281629621,1.0242442580459,1.02420640656117))
REPRESENTATION_ITEM('')
);
#630=(
BOUNDED_CURVE()
B_SPLINE_CURVE(2,(#36960,#36961,#36962),.UNSPECIFIED.,.F.,.F.)
B_SPLINE_CURVE_WITH_KNOTS((3,3),(-0.27009889353462,-0.21874603147717),
 .UNSPECIFIED.)
CURVE()
GEOMETRIC_REPRESENTATION_ITEM()
RATIONAL_B_SPLINE_CURVE((1.02420640656117,1.02306098691693,1.02147610369993))
REPRESENTATION_ITEM('')
);
#631=(
BOUNDED_CURVE()
B_SPLINE_CURVE(2,(#36964,#36965,#36966),.UNSPECIFIED.,.F.,.F.)
B_SPLINE_CURVE_WITH_KNOTS((3,3),(-0.589144372850598,-0.536094506482415),
 .UNSPECIFIED.)
CURVE()
GEOMETRIC_REPRESENTATION_ITEM()
RATIONAL_B_SPLINE_CURVE((1.02147610369988,1.02311336089455,1.02428162962093))
REPRESENTATION_ITEM('')
);
#632=(
BOUNDED_CURVE()
B_SPLINE_CURVE(2,(#36970,#36971,#36972),.UNSPECIFIED.,.F.,.F.)
B_SPLINE_CURVE_WITH_KNOTS((3,3),(-0.271795897845352,-0.218746031477165),
 .UNSPECIFIED.)
CURVE()
GEOMETRIC_REPRESENTATION_ITEM()
RATIONAL_B_SPLINE_CURVE((1.02428162962101,1.02311336089462,1.02147610369994))
REPRESENTATION_ITEM('')
);
#633=(
BOUNDED_CURVE()
B_SPLINE_CURVE(2,(#36974,#36975,#36976),.UNSPECIFIED.,.F.,.F.)
B_SPLINE_CURVE_WITH_KNOTS((3,3),(-0.589144372850592,-0.536094506482404),
 .UNSPECIFIED.)
CURVE()
GEOMETRIC_REPRESENTATION_ITEM()
RATIONAL_B_SPLINE_CURVE((1.02147610369997,1.02311336089465,1.02428162962104))
REPRESENTATION_ITEM('')
);
#634=(
BOUNDED_CURVE()
B_SPLINE_CURVE(2,(#36980,#36981,#36982),.UNSPECIFIED.,.F.,.F.)
B_SPLINE_CURVE_WITH_KNOTS((3,3),(-0.27179589784535,-0.218746031477166),
 .UNSPECIFIED.)
CURVE()
GEOMETRIC_REPRESENTATION_ITEM()
RATIONAL_B_SPLINE_CURVE((1.02428162962095,1.02311336089456,1.02147610369989))
REPRESENTATION_ITEM('')
);
#635=(
BOUNDED_CURVE()
B_SPLINE_CURVE(2,(#36984,#36985,#36986),.UNSPECIFIED.,.F.,.F.)
B_SPLINE_CURVE_WITH_KNOTS((3,3),(-0.589144372850593,-0.536094506482409),
 .UNSPECIFIED.)
CURVE()
GEOMETRIC_REPRESENTATION_ITEM()
RATIONAL_B_SPLINE_CURVE((1.02147610369989,1.02311336089456,1.02428162962095))
REPRESENTATION_ITEM('')
);
#636=(
BOUNDED_CURVE()
B_SPLINE_CURVE(2,(#36990,#36991,#36992),.UNSPECIFIED.,.F.,.F.)
B_SPLINE_CURVE_WITH_KNOTS((3,3),(-0.27179589784535,-0.218746031477166),
 .UNSPECIFIED.)
CURVE()
GEOMETRIC_REPRESENTATION_ITEM()
RATIONAL_B_SPLINE_CURVE((1.02428162962097,1.02311336089458,1.02147610369991))
REPRESENTATION_ITEM('')
);
#637=(
BOUNDED_CURVE()
B_SPLINE_CURVE(2,(#36994,#36995,#36996),.UNSPECIFIED.,.F.,.F.)
B_SPLINE_CURVE_WITH_KNOTS((3,3),(-0.589144372850588,-0.536094506482405),
 .UNSPECIFIED.)
CURVE()
GEOMETRIC_REPRESENTATION_ITEM()
RATIONAL_B_SPLINE_CURVE((1.02147610369989,1.02311336089456,1.02428162962095))
REPRESENTATION_ITEM('')
);
#638=(
BOUNDED_CURVE()
B_SPLINE_CURVE(2,(#37000,#37001,#37002),.UNSPECIFIED.,.F.,.F.)
B_SPLINE_CURVE_WITH_KNOTS((3,3),(-0.271795897845364,-0.218746031477175),
 .UNSPECIFIED.)
CURVE()
GEOMETRIC_REPRESENTATION_ITEM()
RATIONAL_B_SPLINE_CURVE((1.02428162962103,1.02311336089464,1.02147610369996))
REPRESENTATION_ITEM('')
);
#639=(
BOUNDED_CURVE()
B_SPLINE_CURVE(2,(#37004,#37005,#37006),.UNSPECIFIED.,.F.,.F.)
B_SPLINE_CURVE_WITH_KNOTS((3,3),(-0.589144372850586,-0.5360945064824),
 .UNSPECIFIED.)
CURVE()
GEOMETRIC_REPRESENTATION_ITEM()
RATIONAL_B_SPLINE_CURVE((1.02147610369993,1.0231133608946,1.02428162962099))
REPRESENTATION_ITEM('')
);
#640=(
BOUNDED_CURVE()
B_SPLINE_CURVE(2,(#37010,#37011,#37012),.UNSPECIFIED.,.F.,.F.)
B_SPLINE_CURVE_WITH_KNOTS((3,3),(-0.271795897845344,-0.218746031477157),
 .UNSPECIFIED.)
CURVE()
GEOMETRIC_REPRESENTATION_ITEM()
RATIONAL_B_SPLINE_CURVE((1.02428162962104,1.02311336089464,1.02147610369997))
REPRESENTATION_ITEM('')
);
#641=(
BOUNDED_CURVE()
B_SPLINE_CURVE(2,(#37014,#37015,#37016),.UNSPECIFIED.,.F.,.F.)
B_SPLINE_CURVE_WITH_KNOTS((3,3),(-0.589144372850594,-0.536094506482411),
 .UNSPECIFIED.)
CURVE()
GEOMETRIC_REPRESENTATION_ITEM()
RATIONAL_B_SPLINE_CURVE((1.02147610369987,1.02311336089454,1.02428162962093))
REPRESENTATION_ITEM('')
);
#642=(
BOUNDED_CURVE()
B_SPLINE_CURVE(2,(#37020,#37021,#37022),.UNSPECIFIED.,.F.,.F.)
B_SPLINE_CURVE_WITH_KNOTS((3,3),(-0.271795897845363,-0.218746031477177),
 .UNSPECIFIED.)
CURVE()
GEOMETRIC_REPRESENTATION_ITEM()
RATIONAL_B_SPLINE_CURVE((1.02428162962096,1.02311336089457,1.0214761036999))
REPRESENTATION_ITEM('')
);
#643=(
BOUNDED_CURVE()
B_SPLINE_CURVE(2,(#37024,#37025,#37026),.UNSPECIFIED.,.F.,.F.)
B_SPLINE_CURVE_WITH_KNOTS((3,3),(-0.589144372850603,-0.536094506482417),
 .UNSPECIFIED.)
CURVE()
GEOMETRIC_REPRESENTATION_ITEM()
RATIONAL_B_SPLINE_CURVE((1.02147610369994,1.02311336089461,1.024281629621))
REPRESENTATION_ITEM('')
);
#644=(
BOUNDED_CURVE()
B_SPLINE_CURVE(2,(#37030,#37031,#37032),.UNSPECIFIED.,.F.,.F.)
B_SPLINE_CURVE_WITH_KNOTS((3,3),(-0.271795897845351,-0.218746031477165),
 .UNSPECIFIED.)
CURVE()
GEOMETRIC_REPRESENTATION_ITEM()
RATIONAL_B_SPLINE_CURVE((1.024281629621,1.02311336089461,1.02147610369993))
REPRESENTATION_ITEM('')
);
#645=(
BOUNDED_CURVE()
B_SPLINE_CURVE(2,(#37034,#37035,#37036),.UNSPECIFIED.,.F.,.F.)
B_SPLINE_CURVE_WITH_KNOTS((3,3),(-0.589144372850587,-0.536094506482401),
 .UNSPECIFIED.)
CURVE()
GEOMETRIC_REPRESENTATION_ITEM()
RATIONAL_B_SPLINE_CURVE((1.02147610369992,1.02311336089459,1.02428162962098))
REPRESENTATION_ITEM('')
);
#646=(
BOUNDED_CURVE()
B_SPLINE_CURVE(2,(#37040,#37041,#37042),.UNSPECIFIED.,.F.,.F.)
B_SPLINE_CURVE_WITH_KNOTS((3,3),(-0.271795897845358,-0.218746031477172),
 .UNSPECIFIED.)
CURVE()
GEOMETRIC_REPRESENTATION_ITEM()
RATIONAL_B_SPLINE_CURVE((1.02428162962097,1.02311336089458,1.02147610369991))
REPRESENTATION_ITEM('')
);
#647=(
BOUNDED_CURVE()
B_SPLINE_CURVE(2,(#37044,#37045,#37046),.UNSPECIFIED.,.F.,.F.)
B_SPLINE_CURVE_WITH_KNOTS((3,3),(-0.589144372850593,-0.536094506482406),
 .UNSPECIFIED.)
CURVE()
GEOMETRIC_REPRESENTATION_ITEM()
RATIONAL_B_SPLINE_CURVE((1.02147610369993,1.02311336089461,1.024281629621))
REPRESENTATION_ITEM('')
);
#648=(
BOUNDED_CURVE()
B_SPLINE_CURVE(2,(#37050,#37051,#37052),.UNSPECIFIED.,.F.,.F.)
B_SPLINE_CURVE_WITH_KNOTS((3,3),(-0.271795897845347,-0.218746031477162),
 .UNSPECIFIED.)
CURVE()
GEOMETRIC_REPRESENTATION_ITEM()
RATIONAL_B_SPLINE_CURVE((1.02428162962098,1.02311336089459,1.02147610369992))
REPRESENTATION_ITEM('')
);
#649=(
BOUNDED_CURVE()
B_SPLINE_CURVE(2,(#37054,#37055,#37056),.UNSPECIFIED.,.F.,.F.)
B_SPLINE_CURVE_WITH_KNOTS((3,3),(-0.5891443728506,-0.536094506482414),
 .UNSPECIFIED.)
CURVE()
GEOMETRIC_REPRESENTATION_ITEM()
RATIONAL_B_SPLINE_CURVE((1.02147610369995,1.02311336089463,1.02428162962102))
REPRESENTATION_ITEM('')
);
#650=(
BOUNDED_CURVE()
B_SPLINE_CURVE(2,(#37060,#37061,#37062),.UNSPECIFIED.,.F.,.F.)
B_SPLINE_CURVE_WITH_KNOTS((3,3),(-0.271795897845356,-0.218746031477171),
 .UNSPECIFIED.)
CURVE()
GEOMETRIC_REPRESENTATION_ITEM()
RATIONAL_B_SPLINE_CURVE((1.02428162962096,1.02311336089457,1.0214761036999))
REPRESENTATION_ITEM('')
);
#651=(
BOUNDED_CURVE()
B_SPLINE_CURVE(2,(#37064,#37065,#37066),.UNSPECIFIED.,.F.,.F.)
B_SPLINE_CURVE_WITH_KNOTS((3,3),(-0.589144372850587,-0.536094506482402),
 .UNSPECIFIED.)
CURVE()
GEOMETRIC_REPRESENTATION_ITEM()
RATIONAL_B_SPLINE_CURVE((1.02147610369992,1.02311336089459,1.02428162962098))
REPRESENTATION_ITEM('')
);
#652=(
BOUNDED_CURVE()
B_SPLINE_CURVE(2,(#37070,#37071,#37072),.UNSPECIFIED.,.F.,.F.)
B_SPLINE_CURVE_WITH_KNOTS((3,3),(-0.271795897845355,-0.21874603147717),
 .UNSPECIFIED.)
CURVE()
GEOMETRIC_REPRESENTATION_ITEM()
RATIONAL_B_SPLINE_CURVE((1.02428162962097,1.02311336089458,1.0214761036999))
REPRESENTATION_ITEM('')
);
#653=(
BOUNDED_CURVE()
B_SPLINE_CURVE(2,(#37074,#37075,#37076),.UNSPECIFIED.,.F.,.F.)
B_SPLINE_CURVE_WITH_KNOTS((3,3),(-0.589144372850594,-0.53609450648241),
 .UNSPECIFIED.)
CURVE()
GEOMETRIC_REPRESENTATION_ITEM()
RATIONAL_B_SPLINE_CURVE((1.0214761036999,1.02311336089457,1.02428162962096))
REPRESENTATION_ITEM('')
);
#654=(
BOUNDED_CURVE()
B_SPLINE_CURVE(2,(#37080,#37081,#37082),.UNSPECIFIED.,.F.,.F.)
B_SPLINE_CURVE_WITH_KNOTS((3,3),(-0.271795897845353,-0.218746031477171),
 .UNSPECIFIED.)
CURVE()
GEOMETRIC_REPRESENTATION_ITEM()
RATIONAL_B_SPLINE_CURVE((1.02428162962091,1.02311336089453,1.02147610369986))
REPRESENTATION_ITEM('')
);
#655=(
BOUNDED_CURVE()
B_SPLINE_CURVE(2,(#37084,#37085,#37086),.UNSPECIFIED.,.F.,.F.)
B_SPLINE_CURVE_WITH_KNOTS((3,3),(-0.589144372850593,-0.536094506482411),
 .UNSPECIFIED.)
CURVE()
GEOMETRIC_REPRESENTATION_ITEM()
RATIONAL_B_SPLINE_CURVE((1.02147610369985,1.02311336089452,1.0242816296209))
REPRESENTATION_ITEM('')
);
#656=(
BOUNDED_CURVE()
B_SPLINE_CURVE(2,(#37090,#37091,#37092),.UNSPECIFIED.,.F.,.F.)
B_SPLINE_CURVE_WITH_KNOTS((3,3),(-0.27179589784535,-0.218746031477166),
 .UNSPECIFIED.)
CURVE()
GEOMETRIC_REPRESENTATION_ITEM()
RATIONAL_B_SPLINE_CURVE((1.02428162962095,1.02311336089457,1.02147610369989))
REPRESENTATION_ITEM('')
);
#657=(
BOUNDED_CURVE()
B_SPLINE_CURVE(2,(#37094,#37095,#37096),.UNSPECIFIED.,.F.,.F.)
B_SPLINE_CURVE_WITH_KNOTS((3,3),(-0.589144372850597,-0.536094506482411),
 .UNSPECIFIED.)
CURVE()
GEOMETRIC_REPRESENTATION_ITEM()
RATIONAL_B_SPLINE_CURVE((1.02147610369993,1.0231133608946,1.02428162962099))
REPRESENTATION_ITEM('')
);
#658=(
BOUNDED_CURVE()
B_SPLINE_CURVE(2,(#37100,#37101,#37102),.UNSPECIFIED.,.F.,.F.)
B_SPLINE_CURVE_WITH_KNOTS((3,3),(-0.271795897845352,-0.218746031477167),
 .UNSPECIFIED.)
CURVE()
GEOMETRIC_REPRESENTATION_ITEM()
RATIONAL_B_SPLINE_CURVE((1.02428162962097,1.02311336089458,1.02147610369991))
REPRESENTATION_ITEM('')
);
#659=(
BOUNDED_CURVE()
B_SPLINE_CURVE(2,(#37104,#37105,#37106),.UNSPECIFIED.,.F.,.F.)
B_SPLINE_CURVE_WITH_KNOTS((3,3),(-0.589144372850601,-0.536094506482415),
 .UNSPECIFIED.)
CURVE()
GEOMETRIC_REPRESENTATION_ITEM()
RATIONAL_B_SPLINE_CURVE((1.02147610369994,1.02311336089461,1.024281629621))
REPRESENTATION_ITEM('')
);
#660=(
BOUNDED_CURVE()
B_SPLINE_CURVE(2,(#37110,#37111,#37112),.UNSPECIFIED.,.F.,.F.)
B_SPLINE_CURVE_WITH_KNOTS((3,3),(-0.271795897845354,-0.21874603147717),
 .UNSPECIFIED.)
CURVE()
GEOMETRIC_REPRESENTATION_ITEM()
RATIONAL_B_SPLINE_CURVE((1.02428162962094,1.02311336089455,1.02147610369988))
REPRESENTATION_ITEM('')
);
#661=(
BOUNDED_CURVE()
B_SPLINE_CURVE(2,(#37114,#37115,#37116),.UNSPECIFIED.,.F.,.F.)
B_SPLINE_CURVE_WITH_KNOTS((3,3),(-0.589144372850587,-0.536094506482405),
 .UNSPECIFIED.)
CURVE()
GEOMETRIC_REPRESENTATION_ITEM()
RATIONAL_B_SPLINE_CURVE((1.02147610369984,1.02311336089451,1.02428162962089))
REPRESENTATION_ITEM('')
);
#662=(
BOUNDED_CURVE()
B_SPLINE_CURVE(2,(#37120,#37121,#37122),.UNSPECIFIED.,.F.,.F.)
B_SPLINE_CURVE_WITH_KNOTS((3,3),(-0.271795897845346,-0.218746031477161),
 .UNSPECIFIED.)
CURVE()
GEOMETRIC_REPRESENTATION_ITEM()
RATIONAL_B_SPLINE_CURVE((1.02428162962098,1.02311336089459,1.02147610369992))
REPRESENTATION_ITEM('')
);
#663=(
BOUNDED_CURVE()
B_SPLINE_CURVE(2,(#37124,#37125,#37126),.UNSPECIFIED.,.F.,.F.)
B_SPLINE_CURVE_WITH_KNOTS((3,3),(-0.589144372850597,-0.536094506482412),
 .UNSPECIFIED.)
CURVE()
GEOMETRIC_REPRESENTATION_ITEM()
RATIONAL_B_SPLINE_CURVE((1.02147610369992,1.02311336089459,1.02428162962098))
REPRESENTATION_ITEM('')
);
#664=(
BOUNDED_CURVE()
B_SPLINE_CURVE(2,(#37130,#37131,#37132),.UNSPECIFIED.,.F.,.F.)
B_SPLINE_CURVE_WITH_KNOTS((3,3),(-0.271795897845346,-0.218746031477161),
 .UNSPECIFIED.)
CURVE()
GEOMETRIC_REPRESENTATION_ITEM()
RATIONAL_B_SPLINE_CURVE((1.02428162962099,1.0231133608946,1.02147610369993))
REPRESENTATION_ITEM('')
);
#665=(
BOUNDED_CURVE()
B_SPLINE_CURVE(2,(#37134,#37135,#37136),.UNSPECIFIED.,.F.,.F.)
B_SPLINE_CURVE_WITH_KNOTS((3,3),(-0.589144372850585,-0.536094506482398),
 .UNSPECIFIED.)
CURVE()
GEOMETRIC_REPRESENTATION_ITEM()
RATIONAL_B_SPLINE_CURVE((1.02147610369994,1.02311336089461,1.024281629621))
REPRESENTATION_ITEM('')
);
#666=(
BOUNDED_CURVE()
B_SPLINE_CURVE(2,(#37140,#37141,#37142),.UNSPECIFIED.,.F.,.F.)
B_SPLINE_CURVE_WITH_KNOTS((3,3),(-0.271795897845348,-0.218746031477163),
 .UNSPECIFIED.)
CURVE()
GEOMETRIC_REPRESENTATION_ITEM()
RATIONAL_B_SPLINE_CURVE((1.02428162962098,1.02311336089459,1.02147610369992))
REPRESENTATION_ITEM('')
);
#667=(
BOUNDED_CURVE()
B_SPLINE_CURVE(2,(#37144,#37145,#37146),.UNSPECIFIED.,.F.,.F.)
B_SPLINE_CURVE_WITH_KNOTS((3,3),(-0.589144372850599,-0.536094506482412),
 .UNSPECIFIED.)
CURVE()
GEOMETRIC_REPRESENTATION_ITEM()
RATIONAL_B_SPLINE_CURVE((1.02147610369994,1.02311336089462,1.02428162962101))
REPRESENTATION_ITEM('')
);
#668=(
BOUNDED_CURVE()
B_SPLINE_CURVE(2,(#37150,#37151,#37152),.UNSPECIFIED.,.F.,.F.)
B_SPLINE_CURVE_WITH_KNOTS((3,3),(-0.271795897845354,-0.21874603147717),
 .UNSPECIFIED.)
CURVE()
GEOMETRIC_REPRESENTATION_ITEM()
RATIONAL_B_SPLINE_CURVE((1.02428162962095,1.02311336089456,1.02147610369989))
REPRESENTATION_ITEM('')
);
#669=(
BOUNDED_CURVE()
B_SPLINE_CURVE(2,(#37154,#37155,#37156),.UNSPECIFIED.,.F.,.F.)
B_SPLINE_CURVE_WITH_KNOTS((3,3),(-0.589144372850593,-0.536094506482408),
 .UNSPECIFIED.)
CURVE()
GEOMETRIC_REPRESENTATION_ITEM()
RATIONAL_B_SPLINE_CURVE((1.0214761036999,1.02311336089457,1.02428162962096))
REPRESENTATION_ITEM('')
);
#670=(
BOUNDED_CURVE()
B_SPLINE_CURVE(2,(#37160,#37161,#37162),.UNSPECIFIED.,.F.,.F.)
B_SPLINE_CURVE_WITH_KNOTS((3,3),(-0.271795897845352,-0.218746031477169),
 .UNSPECIFIED.)
CURVE()
GEOMETRIC_REPRESENTATION_ITEM()
RATIONAL_B_SPLINE_CURVE((1.02428162962095,1.02311336089456,1.02147610369989))
REPRESENTATION_ITEM('')
);
#671=(
BOUNDED_CURVE()
B_SPLINE_CURVE(2,(#37164,#37165,#37166),.UNSPECIFIED.,.F.,.F.)
B_SPLINE_CURVE_WITH_KNOTS((3,3),(-0.589144372850587,-0.536094506482401),
 .UNSPECIFIED.)
CURVE()
GEOMETRIC_REPRESENTATION_ITEM()
RATIONAL_B_SPLINE_CURVE((1.02147610369991,1.02311336089458,1.02428162962097))
REPRESENTATION_ITEM('')
);
#672=(
BOUNDED_CURVE()
B_SPLINE_CURVE(2,(#37170,#37171,#37172),.UNSPECIFIED.,.F.,.F.)
B_SPLINE_CURVE_WITH_KNOTS((3,3),(-0.271795897845353,-0.218746031477167),
 .UNSPECIFIED.)
CURVE()
GEOMETRIC_REPRESENTATION_ITEM()
RATIONAL_B_SPLINE_CURVE((1.02428162962099,1.0231133608946,1.02147610369993))
REPRESENTATION_ITEM('')
);
#673=(
BOUNDED_CURVE()
B_SPLINE_CURVE(2,(#37174,#37175,#37176),.UNSPECIFIED.,.F.,.F.)
B_SPLINE_CURVE_WITH_KNOTS((3,3),(-0.589144372850597,-0.536094506482414),
 .UNSPECIFIED.)
CURVE()
GEOMETRIC_REPRESENTATION_ITEM()
RATIONAL_B_SPLINE_CURVE((1.02147610369988,1.02311336089455,1.02428162962094))
REPRESENTATION_ITEM('')
);
#674=(
BOUNDED_CURVE()
B_SPLINE_CURVE(2,(#37180,#37181,#37182),.UNSPECIFIED.,.F.,.F.)
B_SPLINE_CURVE_WITH_KNOTS((3,3),(-0.271795897845353,-0.218746031477168),
 .UNSPECIFIED.)
CURVE()
GEOMETRIC_REPRESENTATION_ITEM()
RATIONAL_B_SPLINE_CURVE((1.02428162962097,1.02311336089458,1.02147610369991))
REPRESENTATION_ITEM('')
);
#675=(
BOUNDED_CURVE()
B_SPLINE_CURVE(2,(#37184,#37185,#37186),.UNSPECIFIED.,.F.,.F.)
B_SPLINE_CURVE_WITH_KNOTS((3,3),(-0.589144372850594,-0.536094506482409),
 .UNSPECIFIED.)
CURVE()
GEOMETRIC_REPRESENTATION_ITEM()
RATIONAL_B_SPLINE_CURVE((1.02147610369993,1.0231133608946,1.024281629621))
REPRESENTATION_ITEM('')
);
#676=(
BOUNDED_CURVE()
B_SPLINE_CURVE(2,(#37190,#37191,#37192),.UNSPECIFIED.,.F.,.F.)
B_SPLINE_CURVE_WITH_KNOTS((3,3),(-0.271795897845345,-0.21874603147716),
 .UNSPECIFIED.)
CURVE()
GEOMETRIC_REPRESENTATION_ITEM()
RATIONAL_B_SPLINE_CURVE((1.02428162962099,1.0231133608946,1.02147610369993))
REPRESENTATION_ITEM('')
);
#677=(
BOUNDED_CURVE()
B_SPLINE_CURVE(2,(#37194,#37195,#37196),.UNSPECIFIED.,.F.,.F.)
B_SPLINE_CURVE_WITH_KNOTS((3,3),(-0.589144372850594,-0.536094506482408),
 .UNSPECIFIED.)
CURVE()
GEOMETRIC_REPRESENTATION_ITEM()
RATIONAL_B_SPLINE_CURVE((1.02147610369992,1.0231133608946,1.02428162962099))
REPRESENTATION_ITEM('')
);
#678=(
BOUNDED_CURVE()
B_SPLINE_CURVE(2,(#37200,#37201,#37202),.UNSPECIFIED.,.F.,.F.)
B_SPLINE_CURVE_WITH_KNOTS((3,3),(-0.271795897845356,-0.218746031477171),
 .UNSPECIFIED.)
CURVE()
GEOMETRIC_REPRESENTATION_ITEM()
RATIONAL_B_SPLINE_CURVE((1.02428162962096,1.02311336089457,1.0214761036999))
REPRESENTATION_ITEM('')
);
#679=(
BOUNDED_CURVE()
B_SPLINE_CURVE(2,(#37204,#37205,#37206),.UNSPECIFIED.,.F.,.F.)
B_SPLINE_CURVE_WITH_KNOTS((3,3),(-0.58914437285058,-0.536094506482397),
 .UNSPECIFIED.)
CURVE()
GEOMETRIC_REPRESENTATION_ITEM()
RATIONAL_B_SPLINE_CURVE((1.02147610369986,1.02311336089452,1.02428162962091))
REPRESENTATION_ITEM('')
);
#680=(
BOUNDED_CURVE()
B_SPLINE_CURVE(2,(#37210,#37211,#37212),.UNSPECIFIED.,.F.,.F.)
B_SPLINE_CURVE_WITH_KNOTS((3,3),(-0.271795897845352,-0.218746031477169),
 .UNSPECIFIED.)
CURVE()
GEOMETRIC_REPRESENTATION_ITEM()
RATIONAL_B_SPLINE_CURVE((1.02428162962094,1.02311336089455,1.02147610369988))
REPRESENTATION_ITEM('')
);
#681=(
BOUNDED_CURVE()
B_SPLINE_CURVE(2,(#37214,#37215,#37216),.UNSPECIFIED.,.F.,.F.)
B_SPLINE_CURVE_WITH_KNOTS((3,3),(-0.589144372850582,-0.536094506482401),
 .UNSPECIFIED.)
CURVE()
GEOMETRIC_REPRESENTATION_ITEM()
RATIONAL_B_SPLINE_CURVE((1.02147610369982,1.02311336089448,1.02428162962087))
REPRESENTATION_ITEM('')
);
#682=(
BOUNDED_CURVE()
B_SPLINE_CURVE(2,(#37220,#37221,#37222),.UNSPECIFIED.,.F.,.F.)
B_SPLINE_CURVE_WITH_KNOTS((3,3),(-0.271795897845355,-0.218746031477168),
 .UNSPECIFIED.)
CURVE()
GEOMETRIC_REPRESENTATION_ITEM()
RATIONAL_B_SPLINE_CURVE((1.02428162962102,1.02311336089462,1.02147610369995))
REPRESENTATION_ITEM('')
);
#683=(
BOUNDED_CURVE()
B_SPLINE_CURVE(2,(#37224,#37225,#37226),.UNSPECIFIED.,.F.,.F.)
B_SPLINE_CURVE_WITH_KNOTS((3,3),(-0.589144372850599,-0.536094506482414),
 .UNSPECIFIED.)
CURVE()
GEOMETRIC_REPRESENTATION_ITEM()
RATIONAL_B_SPLINE_CURVE((1.02147610369993,1.0231133608946,1.02428162962099))
REPRESENTATION_ITEM('')
);
#684=(
BOUNDED_CURVE()
B_SPLINE_CURVE(2,(#37230,#37231,#37232),.UNSPECIFIED.,.F.,.F.)
B_SPLINE_CURVE_WITH_KNOTS((3,3),(-0.271795897845353,-0.218746031477169),
 .UNSPECIFIED.)
CURVE()
GEOMETRIC_REPRESENTATION_ITEM()
RATIONAL_B_SPLINE_CURVE((1.02428162962096,1.02311336089457,1.0214761036999))
REPRESENTATION_ITEM('')
);
#685=(
BOUNDED_CURVE()
B_SPLINE_CURVE(2,(#37234,#37235,#37236),.UNSPECIFIED.,.F.,.F.)
B_SPLINE_CURVE_WITH_KNOTS((3,3),(-0.589144372850601,-0.536094506482415),
 .UNSPECIFIED.)
CURVE()
GEOMETRIC_REPRESENTATION_ITEM()
RATIONAL_B_SPLINE_CURVE((1.02147610369991,1.02311336089458,1.02428162962097))
REPRESENTATION_ITEM('')
);
#686=(
BOUNDED_CURVE()
B_SPLINE_CURVE(2,(#37240,#37241,#37242),.UNSPECIFIED.,.F.,.F.)
B_SPLINE_CURVE_WITH_KNOTS((3,3),(-0.271795897845357,-0.218746031477176),
 .UNSPECIFIED.)
CURVE()
GEOMETRIC_REPRESENTATION_ITEM()
RATIONAL_B_SPLINE_CURVE((1.02428162962087,1.02311336089448,1.02147610369982))
REPRESENTATION_ITEM('')
);
#687=(
BOUNDED_CURVE()
B_SPLINE_CURVE(2,(#37244,#37245,#37246),.UNSPECIFIED.,.F.,.F.)
B_SPLINE_CURVE_WITH_KNOTS((3,3),(-0.589144372850592,-0.536094506482409),
 .UNSPECIFIED.)
CURVE()
GEOMETRIC_REPRESENTATION_ITEM()
RATIONAL_B_SPLINE_CURVE((1.02147610369983,1.0231133608945,1.02428162962089))
REPRESENTATION_ITEM('')
);
#688=(
BOUNDED_CURVE()
B_SPLINE_CURVE(2,(#37250,#37251,#37252),.UNSPECIFIED.,.F.,.F.)
B_SPLINE_CURVE_WITH_KNOTS((3,3),(-0.271795897845353,-0.218746031477169),
 .UNSPECIFIED.)
CURVE()
GEOMETRIC_REPRESENTATION_ITEM()
RATIONAL_B_SPLINE_CURVE((1.02428162962096,1.02311336089457,1.0214761036999))
REPRESENTATION_ITEM('')
);
#689=(
BOUNDED_CURVE()
B_SPLINE_CURVE(2,(#37254,#37255,#37256),.UNSPECIFIED.,.F.,.F.)
B_SPLINE_CURVE_WITH_KNOTS((3,3),(-0.589144372850606,-0.536094506482418),
 .UNSPECIFIED.)
CURVE()
GEOMETRIC_REPRESENTATION_ITEM()
RATIONAL_B_SPLINE_CURVE((1.02147610369997,1.02311336089464,1.02428162962104))
REPRESENTATION_ITEM('')
);
#690=(
BOUNDED_CURVE()
B_SPLINE_CURVE(2,(#37260,#37261,#37262),.UNSPECIFIED.,.F.,.F.)
B_SPLINE_CURVE_WITH_KNOTS((3,3),(-0.271795897845354,-0.218746031477167),
 .UNSPECIFIED.)
CURVE()
GEOMETRIC_REPRESENTATION_ITEM()
RATIONAL_B_SPLINE_CURVE((1.02428162962102,1.02311336089463,1.02147610369995))
REPRESENTATION_ITEM('')
);
#691=(
BOUNDED_CURVE()
B_SPLINE_CURVE(2,(#37264,#37265,#37266),.UNSPECIFIED.,.F.,.F.)
B_SPLINE_CURVE_WITH_KNOTS((3,3),(-0.589144372850594,-0.536094506482407),
 .UNSPECIFIED.)
CURVE()
GEOMETRIC_REPRESENTATION_ITEM()
RATIONAL_B_SPLINE_CURVE((1.02147610369996,1.02311336089464,1.02428162962103))
REPRESENTATION_ITEM('')
);
#692=(
BOUNDED_CURVE()
B_SPLINE_CURVE(2,(#37270,#37271,#37272),.UNSPECIFIED.,.F.,.F.)
B_SPLINE_CURVE_WITH_KNOTS((3,3),(-0.271795897845348,-0.218746031477164),
 .UNSPECIFIED.)
CURVE()
GEOMETRIC_REPRESENTATION_ITEM()
RATIONAL_B_SPLINE_CURVE((1.02428162962097,1.02311336089458,1.02147610369991))
REPRESENTATION_ITEM('')
);
#693=(
BOUNDED_CURVE()
B_SPLINE_CURVE(2,(#37274,#37275,#37276),.UNSPECIFIED.,.F.,.F.)
B_SPLINE_CURVE_WITH_KNOTS((3,3),(-0.58914437285059,-0.536094506482404),
 .UNSPECIFIED.)
CURVE()
GEOMETRIC_REPRESENTATION_ITEM()
RATIONAL_B_SPLINE_CURVE((1.02147610369992,1.0231133608946,1.02428162962099))
REPRESENTATION_ITEM('')
);
#694=(
BOUNDED_CURVE()
B_SPLINE_CURVE(2,(#37280,#37281,#37282),.UNSPECIFIED.,.F.,.F.)
B_SPLINE_CURVE_WITH_KNOTS((3,3),(-0.271795897845347,-0.218746031477164),
 .UNSPECIFIED.)
CURVE()
GEOMETRIC_REPRESENTATION_ITEM()
RATIONAL_B_SPLINE_CURVE((1.02428162962094,1.02311336089455,1.02147610369988))
REPRESENTATION_ITEM('')
);
#695=(
BOUNDED_CURVE()
B_SPLINE_CURVE(2,(#37284,#37285,#37286),.UNSPECIFIED.,.F.,.F.)
B_SPLINE_CURVE_WITH_KNOTS((3,3),(-0.589144372850593,-0.536094506482406),
 .UNSPECIFIED.)
CURVE()
GEOMETRIC_REPRESENTATION_ITEM()
RATIONAL_B_SPLINE_CURVE((1.02147610369994,1.02311336089461,1.024281629621))
REPRESENTATION_ITEM('')
);
#696=(
BOUNDED_CURVE()
B_SPLINE_CURVE(2,(#37290,#37291,#37292),.UNSPECIFIED.,.F.,.F.)
B_SPLINE_CURVE_WITH_KNOTS((3,3),(-0.271795897845356,-0.218746031477165),
 .UNSPECIFIED.)
CURVE()
GEOMETRIC_REPRESENTATION_ITEM()
RATIONAL_B_SPLINE_CURVE((1.02428162962109,1.02311336089469,1.02147610370001))
REPRESENTATION_ITEM('')
);
#697=(
BOUNDED_CURVE()
B_SPLINE_CURVE(2,(#37294,#37295,#37296),.UNSPECIFIED.,.F.,.F.)
B_SPLINE_CURVE_WITH_KNOTS((3,3),(-0.589144372850608,-0.536094506482421),
 .UNSPECIFIED.)
CURVE()
GEOMETRIC_REPRESENTATION_ITEM()
RATIONAL_B_SPLINE_CURVE((1.02147610369995,1.02311336089463,1.02428162962102))
REPRESENTATION_ITEM('')
);
#698=(
BOUNDED_CURVE()
B_SPLINE_CURVE(2,(#37300,#37301,#37302),.UNSPECIFIED.,.F.,.F.)
B_SPLINE_CURVE_WITH_KNOTS((3,3),(-0.271795897845346,-0.218746031477161),
 .UNSPECIFIED.)
CURVE()
GEOMETRIC_REPRESENTATION_ITEM()
RATIONAL_B_SPLINE_CURVE((1.02428162962098,1.02311336089459,1.02147610369992))
REPRESENTATION_ITEM('')
);
#699=(
BOUNDED_CURVE()
B_SPLINE_CURVE(2,(#37304,#37305,#37306),.UNSPECIFIED.,.F.,.F.)
B_SPLINE_CURVE_WITH_KNOTS((3,3),(-0.589144372850605,-0.536094506482414),
 .UNSPECIFIED.)
CURVE()
GEOMETRIC_REPRESENTATION_ITEM()
RATIONAL_B_SPLINE_CURVE((1.02147610370001,1.02311336089469,1.02428162962109))
REPRESENTATION_ITEM('')
);
#700=(
BOUNDED_CURVE()
B_SPLINE_CURVE(2,(#37310,#37311,#37312),.UNSPECIFIED.,.F.,.F.)
B_SPLINE_CURVE_WITH_KNOTS((3,3),(-0.271795897845354,-0.218746031477166),
 .UNSPECIFIED.)
CURVE()
GEOMETRIC_REPRESENTATION_ITEM()
RATIONAL_B_SPLINE_CURVE((1.02428162962102,1.02311336089463,1.02147610369995))
REPRESENTATION_ITEM('')
);
#701=(
BOUNDED_CURVE()
B_SPLINE_CURVE(2,(#37314,#37315,#37316),.UNSPECIFIED.,.F.,.F.)
B_SPLINE_CURVE_WITH_KNOTS((3,3),(-0.589144372850611,-0.536094506482426),
 .UNSPECIFIED.)
CURVE()
GEOMETRIC_REPRESENTATION_ITEM()
RATIONAL_B_SPLINE_CURVE((1.0214761036999,1.02311336089457,1.02428162962096))
REPRESENTATION_ITEM('')
);
#702=(
BOUNDED_CURVE()
B_SPLINE_CURVE(2,(#37320,#37321,#37322),.UNSPECIFIED.,.F.,.F.)
B_SPLINE_CURVE_WITH_KNOTS((3,3),(-0.271795897845362,-0.218746031477177),
 .UNSPECIFIED.)
CURVE()
GEOMETRIC_REPRESENTATION_ITEM()
RATIONAL_B_SPLINE_CURVE((1.02428162962094,1.02311336089455,1.02147610369988))
REPRESENTATION_ITEM('')
);
#703=(
BOUNDED_CURVE()
B_SPLINE_CURVE(2,(#37324,#37325,#37326),.UNSPECIFIED.,.F.,.F.)
B_SPLINE_CURVE_WITH_KNOTS((3,3),(-0.589144372850586,-0.536094506482399),
 .UNSPECIFIED.)
CURVE()
GEOMETRIC_REPRESENTATION_ITEM()
RATIONAL_B_SPLINE_CURVE((1.02147610369992,1.0231133608946,1.02428162962099))
REPRESENTATION_ITEM('')
);
#704=(
BOUNDED_CURVE()
B_SPLINE_CURVE(2,(#37330,#37331,#37332),.UNSPECIFIED.,.F.,.F.)
B_SPLINE_CURVE_WITH_KNOTS((3,3),(-0.27179589784536,-0.218746031477171),
 .UNSPECIFIED.)
CURVE()
GEOMETRIC_REPRESENTATION_ITEM()
RATIONAL_B_SPLINE_CURVE((1.02428162962107,1.02311336089468,1.0214761037))
REPRESENTATION_ITEM('')
);
#705=(
BOUNDED_CURVE()
B_SPLINE_CURVE(2,(#37334,#37335,#37336),.UNSPECIFIED.,.F.,.F.)
B_SPLINE_CURVE_WITH_KNOTS((3,3),(-0.589144372850591,-0.536094506482411),
 .UNSPECIFIED.)
CURVE()
GEOMETRIC_REPRESENTATION_ITEM()
RATIONAL_B_SPLINE_CURVE((1.02147610369983,1.02311336089449,1.02428162962088))
REPRESENTATION_ITEM('')
);
#706=(
BOUNDED_CURVE()
B_SPLINE_CURVE(2,(#37339,#37340,#37341),.UNSPECIFIED.,.F.,.F.)
B_SPLINE_CURVE_WITH_KNOTS((3,3),(-0.271795897845348,-0.21874603147716),
 .UNSPECIFIED.)
CURVE()
GEOMETRIC_REPRESENTATION_ITEM()
RATIONAL_B_SPLINE_CURVE((1.02428162962105,1.02311336089466,1.02147610369998))
REPRESENTATION_ITEM('')
);
#707=(
BOUNDED_CURVE()
B_SPLINE_CURVE(2,(#37345,#37346,#37347),.UNSPECIFIED.,.F.,.F.)
B_SPLINE_CURVE_WITH_KNOTS((3,3),(0.536094506482406,0.589144372850591),
 .UNSPECIFIED.)
CURVE()
GEOMETRIC_REPRESENTATION_ITEM()
RATIONAL_B_SPLINE_CURVE((1.02428162962096,1.02311336089457,1.0214761036999))
REPRESENTATION_ITEM('')
);
#708=(
BOUNDED_CURVE()
B_SPLINE_CURVE(2,(#37351,#37352,#37353),.UNSPECIFIED.,.F.,.F.)
B_SPLINE_CURVE_WITH_KNOTS((3,3),(0.218746031477159,0.271795897845346),
 .UNSPECIFIED.)
CURVE()
GEOMETRIC_REPRESENTATION_ITEM()
RATIONAL_B_SPLINE_CURVE((1.02147610369995,1.02311336089463,1.02428162962102))
REPRESENTATION_ITEM('')
);
#709=(
BOUNDED_CURVE()
B_SPLINE_CURVE(2,(#37355,#37356,#37357),.UNSPECIFIED.,.F.,.F.)
B_SPLINE_CURVE_WITH_KNOTS((3,3),(0.536094506482412,0.589144372850603),
 .UNSPECIFIED.)
CURVE()
GEOMETRIC_REPRESENTATION_ITEM()
RATIONAL_B_SPLINE_CURVE((1.02428162962111,1.02311336089471,1.02147610370003))
REPRESENTATION_ITEM('')
);
#710=(
BOUNDED_CURVE()
B_SPLINE_CURVE(2,(#37361,#37362,#37363),.UNSPECIFIED.,.F.,.F.)
B_SPLINE_CURVE_WITH_KNOTS((3,3),(0.218746031477155,0.271795897845339),
 .UNSPECIFIED.)
CURVE()
GEOMETRIC_REPRESENTATION_ITEM()
RATIONAL_B_SPLINE_CURVE((1.02147610369993,1.0231133608946,1.02428162962099))
REPRESENTATION_ITEM('')
);
#711=(
BOUNDED_CURVE()
B_SPLINE_CURVE(2,(#37365,#37366,#37367),.UNSPECIFIED.,.F.,.F.)
B_SPLINE_CURVE_WITH_KNOTS((3,3),(0.536094506482406,0.589144372850597),
 .UNSPECIFIED.)
CURVE()
GEOMETRIC_REPRESENTATION_ITEM()
RATIONAL_B_SPLINE_CURVE((1.02428162962112,1.02311336089472,1.02147610370004))
REPRESENTATION_ITEM('')
);
#712=(
BOUNDED_CURVE()
B_SPLINE_CURVE(2,(#37371,#37372,#37373),.UNSPECIFIED.,.F.,.F.)
B_SPLINE_CURVE_WITH_KNOTS((3,3),(0.218746031477162,0.27179589784535),
 .UNSPECIFIED.)
CURVE()
GEOMETRIC_REPRESENTATION_ITEM()
RATIONAL_B_SPLINE_CURVE((1.02147610369998,1.02311336089466,1.02428162962105))
REPRESENTATION_ITEM('')
);
#713=(
BOUNDED_CURVE()
B_SPLINE_CURVE(2,(#37375,#37376,#37377),.UNSPECIFIED.,.F.,.F.)
B_SPLINE_CURVE_WITH_KNOTS((3,3),(0.536094506482404,0.589144372850595),
 .UNSPECIFIED.)
CURVE()
GEOMETRIC_REPRESENTATION_ITEM()
RATIONAL_B_SPLINE_CURVE((1.02428162962109,1.0231133608947,1.02147610370002))
REPRESENTATION_ITEM('')
);
#714=(
BOUNDED_CURVE()
B_SPLINE_CURVE(2,(#37381,#37382,#37383),.UNSPECIFIED.,.F.,.F.)
B_SPLINE_CURVE_WITH_KNOTS((3,3),(0.218746031477156,0.271795897845341),
 .UNSPECIFIED.)
CURVE()
GEOMETRIC_REPRESENTATION_ITEM()
RATIONAL_B_SPLINE_CURVE((1.02147610369992,1.02311336089459,1.02428162962098))
REPRESENTATION_ITEM('')
);
#715=(
BOUNDED_CURVE()
B_SPLINE_CURVE(2,(#37385,#37386,#37387),.UNSPECIFIED.,.F.,.F.)
B_SPLINE_CURVE_WITH_KNOTS((3,3),(0.536094506482416,0.589144372850602),
 .UNSPECIFIED.)
CURVE()
GEOMETRIC_REPRESENTATION_ITEM()
RATIONAL_B_SPLINE_CURVE((1.02428162962101,1.02311336089462,1.02147610369994))
REPRESENTATION_ITEM('')
);
#716=(
BOUNDED_CURVE()
B_SPLINE_CURVE(2,(#37391,#37392,#37393),.UNSPECIFIED.,.F.,.F.)
B_SPLINE_CURVE_WITH_KNOTS((3,3),(0.218746031477164,0.271795897845351),
 .UNSPECIFIED.)
CURVE()
GEOMETRIC_REPRESENTATION_ITEM()
RATIONAL_B_SPLINE_CURVE((1.02147610369995,1.02311336089463,1.02428162962102))
REPRESENTATION_ITEM('')
);
#717=(
BOUNDED_CURVE()
B_SPLINE_CURVE(2,(#37395,#37396,#37397),.UNSPECIFIED.,.F.,.F.)
B_SPLINE_CURVE_WITH_KNOTS((3,3),(0.536094506482411,0.589144372850598),
 .UNSPECIFIED.)
CURVE()
GEOMETRIC_REPRESENTATION_ITEM()
RATIONAL_B_SPLINE_CURVE((1.024281629621,1.02311336089461,1.02147610369994))
REPRESENTATION_ITEM('')
);
#718=(
BOUNDED_CURVE()
B_SPLINE_CURVE(2,(#37401,#37402,#37403),.UNSPECIFIED.,.F.,.F.)
B_SPLINE_CURVE_WITH_KNOTS((3,3),(0.218746031477161,0.271795897845348),
 .UNSPECIFIED.)
CURVE()
GEOMETRIC_REPRESENTATION_ITEM()
RATIONAL_B_SPLINE_CURVE((1.02147610369997,1.02311336089465,1.02428162962104))
REPRESENTATION_ITEM('')
);
#719=(
BOUNDED_CURVE()
B_SPLINE_CURVE(2,(#37405,#37406,#37407),.UNSPECIFIED.,.F.,.F.)
B_SPLINE_CURVE_WITH_KNOTS((3,3),(0.536094506482405,0.589144372850593),
 .UNSPECIFIED.)
CURVE()
GEOMETRIC_REPRESENTATION_ITEM()
RATIONAL_B_SPLINE_CURVE((1.02428162962104,1.02311336089464,1.02147610369997))
REPRESENTATION_ITEM('')
);
#720=(
BOUNDED_CURVE()
B_SPLINE_CURVE(2,(#37411,#37412,#37413),.UNSPECIFIED.,.F.,.F.)
B_SPLINE_CURVE_WITH_KNOTS((3,3),(0.218746031477169,0.271795897845355),
 .UNSPECIFIED.)
CURVE()
GEOMETRIC_REPRESENTATION_ITEM()
RATIONAL_B_SPLINE_CURVE((1.02147610369994,1.02311336089461,1.02428162962101))
REPRESENTATION_ITEM('')
);
#721=(
BOUNDED_CURVE()
B_SPLINE_CURVE(2,(#37415,#37416,#37417),.UNSPECIFIED.,.F.,.F.)
B_SPLINE_CURVE_WITH_KNOTS((3,3),(0.536094506482416,0.589144372850604),
 .UNSPECIFIED.)
CURVE()
GEOMETRIC_REPRESENTATION_ITEM()
RATIONAL_B_SPLINE_CURVE((1.02428162962105,1.02311336089466,1.02147610369998))
REPRESENTATION_ITEM('')
);
#722=(
BOUNDED_CURVE()
B_SPLINE_CURVE(2,(#37421,#37422,#37423),.UNSPECIFIED.,.F.,.F.)
B_SPLINE_CURVE_WITH_KNOTS((3,3),(0.218746031477159,0.271795897845341),
 .UNSPECIFIED.)
CURVE()
GEOMETRIC_REPRESENTATION_ITEM()
RATIONAL_B_SPLINE_CURVE((1.02147610369987,1.02311336089454,1.02428162962093))
REPRESENTATION_ITEM('')
);
#723=(
BOUNDED_CURVE()
B_SPLINE_CURVE(2,(#37425,#37426,#37427),.UNSPECIFIED.,.F.,.F.)
B_SPLINE_CURVE_WITH_KNOTS((3,3),(0.536094506482407,0.589144372850592),
 .UNSPECIFIED.)
CURVE()
GEOMETRIC_REPRESENTATION_ITEM()
RATIONAL_B_SPLINE_CURVE((1.02428162962098,1.02311336089459,1.02147610369991))
REPRESENTATION_ITEM('')
);
#724=(
BOUNDED_CURVE()
B_SPLINE_CURVE(2,(#37431,#37432,#37433),.UNSPECIFIED.,.F.,.F.)
B_SPLINE_CURVE_WITH_KNOTS((3,3),(0.218746031477156,0.271795897845344),
 .UNSPECIFIED.)
CURVE()
GEOMETRIC_REPRESENTATION_ITEM()
RATIONAL_B_SPLINE_CURVE((1.02147610369997,1.02311336089464,1.02428162962104))
REPRESENTATION_ITEM('')
);
#725=(
BOUNDED_CURVE()
B_SPLINE_CURVE(2,(#37435,#37436,#37437),.UNSPECIFIED.,.F.,.F.)
B_SPLINE_CURVE_WITH_KNOTS((3,3),(0.536094506482407,0.589144372850596),
 .UNSPECIFIED.)
CURVE()
GEOMETRIC_REPRESENTATION_ITEM()
RATIONAL_B_SPLINE_CURVE((1.02428162962105,1.02311336089465,1.02147610369998))
REPRESENTATION_ITEM('')
);
#726=(
BOUNDED_CURVE()
B_SPLINE_CURVE(2,(#37441,#37442,#37443),.UNSPECIFIED.,.F.,.F.)
B_SPLINE_CURVE_WITH_KNOTS((3,3),(0.218746031477169,0.271795897845356),
 .UNSPECIFIED.)
CURVE()
GEOMETRIC_REPRESENTATION_ITEM()
RATIONAL_B_SPLINE_CURVE((1.02147610369994,1.02311336089461,1.024281629621))
REPRESENTATION_ITEM('')
);
#727=(
BOUNDED_CURVE()
B_SPLINE_CURVE(2,(#37445,#37446,#37447),.UNSPECIFIED.,.F.,.F.)
B_SPLINE_CURVE_WITH_KNOTS((3,3),(0.536094506482405,0.589144372850591),
 .UNSPECIFIED.)
CURVE()
GEOMETRIC_REPRESENTATION_ITEM()
RATIONAL_B_SPLINE_CURVE((1.02428162962096,1.02311336089457,1.0214761036999))
REPRESENTATION_ITEM('')
);
#728=(
BOUNDED_CURVE()
B_SPLINE_CURVE(2,(#37451,#37452,#37453),.UNSPECIFIED.,.F.,.F.)
B_SPLINE_CURVE_WITH_KNOTS((3,3),(0.21874603147717,0.271795897845356),
 .UNSPECIFIED.)
CURVE()
GEOMETRIC_REPRESENTATION_ITEM()
RATIONAL_B_SPLINE_CURVE((1.02147610369993,1.0231133608946,1.02428162962099))
REPRESENTATION_ITEM('')
);
#729=(
BOUNDED_CURVE()
B_SPLINE_CURVE(2,(#37455,#37456,#37457),.UNSPECIFIED.,.F.,.F.)
B_SPLINE_CURVE_WITH_KNOTS((3,3),(0.536094506482407,0.589144372850593),
 .UNSPECIFIED.)
CURVE()
GEOMETRIC_REPRESENTATION_ITEM()
RATIONAL_B_SPLINE_CURVE((1.02428162962098,1.02311336089459,1.02147610369992))
REPRESENTATION_ITEM('')
);
#730=(
BOUNDED_CURVE()
B_SPLINE_CURVE(2,(#37461,#37462,#37463),.UNSPECIFIED.,.F.,.F.)
B_SPLINE_CURVE_WITH_KNOTS((3,3),(0.218746031477165,0.271795897845348),
 .UNSPECIFIED.)
CURVE()
GEOMETRIC_REPRESENTATION_ITEM()
RATIONAL_B_SPLINE_CURVE((1.02147610369988,1.02311336089455,1.02428162962093))
REPRESENTATION_ITEM('')
);
#731=(
BOUNDED_CURVE()
B_SPLINE_CURVE(2,(#37465,#37466,#37467),.UNSPECIFIED.,.F.,.F.)
B_SPLINE_CURVE_WITH_KNOTS((3,3),(0.53609450648242,0.589144372850606),
 .UNSPECIFIED.)
CURVE()
GEOMETRIC_REPRESENTATION_ITEM()
RATIONAL_B_SPLINE_CURVE((1.024281629621,1.02311336089461,1.02147610369994))
REPRESENTATION_ITEM('')
);
#732=(
BOUNDED_CURVE()
B_SPLINE_CURVE(2,(#37471,#37472,#37473),.UNSPECIFIED.,.F.,.F.)
B_SPLINE_CURVE_WITH_KNOTS((3,3),(0.218746031477168,0.271795897845355),
 .UNSPECIFIED.)
CURVE()
GEOMETRIC_REPRESENTATION_ITEM()
RATIONAL_B_SPLINE_CURVE((1.02147610369993,1.02311336089461,1.024281629621))
REPRESENTATION_ITEM('')
);
#733=(
BOUNDED_CURVE()
B_SPLINE_CURVE(2,(#37475,#37476,#37477),.UNSPECIFIED.,.F.,.F.)
B_SPLINE_CURVE_WITH_KNOTS((3,3),(0.536094506482407,0.589144372850592),
 .UNSPECIFIED.)
CURVE()
GEOMETRIC_REPRESENTATION_ITEM()
RATIONAL_B_SPLINE_CURVE((1.02428162962095,1.02311336089456,1.02147610369989))
REPRESENTATION_ITEM('')
);
#734=(
BOUNDED_CURVE()
B_SPLINE_CURVE(2,(#37481,#37482,#37483),.UNSPECIFIED.,.F.,.F.)
B_SPLINE_CURVE_WITH_KNOTS((3,3),(0.218746031477166,0.271795897845353),
 .UNSPECIFIED.)
CURVE()
GEOMETRIC_REPRESENTATION_ITEM()
RATIONAL_B_SPLINE_CURVE((1.02147610369992,1.0231133608946,1.02428162962099))
REPRESENTATION_ITEM('')
);
#735=(
BOUNDED_CURVE()
B_SPLINE_CURVE(2,(#37485,#37486,#37487),.UNSPECIFIED.,.F.,.F.)
B_SPLINE_CURVE_WITH_KNOTS((3,3),(0.536094506482401,0.589144372850589),
 .UNSPECIFIED.)
CURVE()
GEOMETRIC_REPRESENTATION_ITEM()
RATIONAL_B_SPLINE_CURVE((1.02428162962102,1.02311336089463,1.02147610369996))
REPRESENTATION_ITEM('')
);
#736=(
BOUNDED_CURVE()
B_SPLINE_CURVE(2,(#37491,#37492,#37493),.UNSPECIFIED.,.F.,.F.)
B_SPLINE_CURVE_WITH_KNOTS((3,3),(0.218746031477163,0.271795897845347),
 .UNSPECIFIED.)
CURVE()
GEOMETRIC_REPRESENTATION_ITEM()
RATIONAL_B_SPLINE_CURVE((1.0214761036999,1.02311336089457,1.02428162962096))
REPRESENTATION_ITEM('')
);
#737=(
BOUNDED_CURVE()
B_SPLINE_CURVE(2,(#37495,#37496,#37497),.UNSPECIFIED.,.F.,.F.)
B_SPLINE_CURVE_WITH_KNOTS((3,3),(0.536094506482403,0.58914437285059),
 .UNSPECIFIED.)
CURVE()
GEOMETRIC_REPRESENTATION_ITEM()
RATIONAL_B_SPLINE_CURVE((1.02428162962101,1.02311336089462,1.02147610369994))
REPRESENTATION_ITEM('')
);
#738=(
BOUNDED_CURVE()
B_SPLINE_CURVE(2,(#37501,#37502,#37503),.UNSPECIFIED.,.F.,.F.)
B_SPLINE_CURVE_WITH_KNOTS((3,3),(0.218746031477163,0.271795897845349),
 .UNSPECIFIED.)
CURVE()
GEOMETRIC_REPRESENTATION_ITEM()
RATIONAL_B_SPLINE_CURVE((1.02147610369993,1.02311336089461,1.024281629621))
REPRESENTATION_ITEM('')
);
#739=(
BOUNDED_CURVE()
B_SPLINE_CURVE(2,(#37505,#37506,#37507),.UNSPECIFIED.,.F.,.F.)
B_SPLINE_CURVE_WITH_KNOTS((3,3),(0.536094506482407,0.589144372850591),
 .UNSPECIFIED.)
CURVE()
GEOMETRIC_REPRESENTATION_ITEM()
RATIONAL_B_SPLINE_CURVE((1.02428162962096,1.02311336089457,1.0214761036999))
REPRESENTATION_ITEM('')
);
#740=(
BOUNDED_CURVE()
B_SPLINE_CURVE(2,(#37511,#37512,#37513),.UNSPECIFIED.,.F.,.F.)
B_SPLINE_CURVE_WITH_KNOTS((3,3),(0.218746031477169,0.271795897845354),
 .UNSPECIFIED.)
CURVE()
GEOMETRIC_REPRESENTATION_ITEM()
RATIONAL_B_SPLINE_CURVE((1.0214761036999,1.02311336089457,1.02428162962096))
REPRESENTATION_ITEM('')
);
#741=(
BOUNDED_CURVE()
B_SPLINE_CURVE(2,(#37515,#37516,#37517),.UNSPECIFIED.,.F.,.F.)
B_SPLINE_CURVE_WITH_KNOTS((3,3),(0.536094506482406,0.589144372850594),
 .UNSPECIFIED.)
CURVE()
GEOMETRIC_REPRESENTATION_ITEM()
RATIONAL_B_SPLINE_CURVE((1.02428162962102,1.02311336089463,1.02147610369995))
REPRESENTATION_ITEM('')
);
#742=(
BOUNDED_CURVE()
B_SPLINE_CURVE(2,(#37521,#37522,#37523),.UNSPECIFIED.,.F.,.F.)
B_SPLINE_CURVE_WITH_KNOTS((3,3),(0.218746031477168,0.271795897845353),
 .UNSPECIFIED.)
CURVE()
GEOMETRIC_REPRESENTATION_ITEM()
RATIONAL_B_SPLINE_CURVE((1.02147610369991,1.02311336089458,1.02428162962097))
REPRESENTATION_ITEM('')
);
#743=(
BOUNDED_CURVE()
B_SPLINE_CURVE(2,(#37525,#37526,#37527),.UNSPECIFIED.,.F.,.F.)
B_SPLINE_CURVE_WITH_KNOTS((3,3),(0.536094506482413,0.589144372850603),
 .UNSPECIFIED.)
CURVE()
GEOMETRIC_REPRESENTATION_ITEM()
RATIONAL_B_SPLINE_CURVE((1.02428162962108,1.02311336089468,1.0214761037))
REPRESENTATION_ITEM('')
);
#744=(
BOUNDED_CURVE()
B_SPLINE_CURVE(2,(#37531,#37532,#37533),.UNSPECIFIED.,.F.,.F.)
B_SPLINE_CURVE_WITH_KNOTS((3,3),(0.218746031477166,0.27179589784535),
 .UNSPECIFIED.)
CURVE()
GEOMETRIC_REPRESENTATION_ITEM()
RATIONAL_B_SPLINE_CURVE((1.02147610369991,1.02311336089458,1.02428162962097))
REPRESENTATION_ITEM('')
);
#745=(
BOUNDED_CURVE()
B_SPLINE_CURVE(2,(#37535,#37536,#37537),.UNSPECIFIED.,.F.,.F.)
B_SPLINE_CURVE_WITH_KNOTS((3,3),(0.536094506482411,0.589144372850594),
 .UNSPECIFIED.)
CURVE()
GEOMETRIC_REPRESENTATION_ITEM()
RATIONAL_B_SPLINE_CURVE((1.02428162962096,1.02311336089457,1.0214761036999))
REPRESENTATION_ITEM('')
);
#746=(
BOUNDED_CURVE()
B_SPLINE_CURVE(2,(#37541,#37542,#37543),.UNSPECIFIED.,.F.,.F.)
B_SPLINE_CURVE_WITH_KNOTS((3,3),(0.218746031477168,0.271795897845354),
 .UNSPECIFIED.)
CURVE()
GEOMETRIC_REPRESENTATION_ITEM()
RATIONAL_B_SPLINE_CURVE((1.02147610369994,1.02311336089461,1.024281629621))
REPRESENTATION_ITEM('')
);
#747=(
BOUNDED_CURVE()
B_SPLINE_CURVE(2,(#37545,#37546,#37547),.UNSPECIFIED.,.F.,.F.)
B_SPLINE_CURVE_WITH_KNOTS((3,3),(0.536094506482396,0.589144372850584),
 .UNSPECIFIED.)
CURVE()
GEOMETRIC_REPRESENTATION_ITEM()
RATIONAL_B_SPLINE_CURVE((1.02428162962101,1.02311336089462,1.02147610369994))
REPRESENTATION_ITEM('')
);
#748=(
BOUNDED_CURVE()
B_SPLINE_CURVE(2,(#37551,#37552,#37553),.UNSPECIFIED.,.F.,.F.)
B_SPLINE_CURVE_WITH_KNOTS((3,3),(0.21874603147717,0.271795897845356),
 .UNSPECIFIED.)
CURVE()
GEOMETRIC_REPRESENTATION_ITEM()
RATIONAL_B_SPLINE_CURVE((1.02147610369993,1.0231133608946,1.024281629621))
REPRESENTATION_ITEM('')
);
#749=(
BOUNDED_CURVE()
B_SPLINE_CURVE(2,(#37555,#37556,#37557),.UNSPECIFIED.,.F.,.F.)
B_SPLINE_CURVE_WITH_KNOTS((3,3),(0.536094506482412,0.589144372850595),
 .UNSPECIFIED.)
CURVE()
GEOMETRIC_REPRESENTATION_ITEM()
RATIONAL_B_SPLINE_CURVE((1.02428162962094,1.02311336089456,1.02147610369989))
REPRESENTATION_ITEM('')
);
#750=(
BOUNDED_CURVE()
B_SPLINE_CURVE(2,(#37561,#37562,#37563),.UNSPECIFIED.,.F.,.F.)
B_SPLINE_CURVE_WITH_KNOTS((3,3),(0.218746031477162,0.271795897845349),
 .UNSPECIFIED.)
CURVE()
GEOMETRIC_REPRESENTATION_ITEM()
RATIONAL_B_SPLINE_CURVE((1.02147610369997,1.02311336089465,1.02428162962104))
REPRESENTATION_ITEM('')
);
#751=(
BOUNDED_CURVE()
B_SPLINE_CURVE(2,(#37565,#37566,#37567),.UNSPECIFIED.,.F.,.F.)
B_SPLINE_CURVE_WITH_KNOTS((3,3),(0.536094506482409,0.589144372850593),
 .UNSPECIFIED.)
CURVE()
GEOMETRIC_REPRESENTATION_ITEM()
RATIONAL_B_SPLINE_CURVE((1.02428162962095,1.02311336089457,1.02147610369989))
REPRESENTATION_ITEM('')
);
#752=(
BOUNDED_CURVE()
B_SPLINE_CURVE(2,(#37571,#37572,#37573),.UNSPECIFIED.,.F.,.F.)
B_SPLINE_CURVE_WITH_KNOTS((3,3),(0.218746031477157,0.271795897845344),
 .UNSPECIFIED.)
CURVE()
GEOMETRIC_REPRESENTATION_ITEM()
RATIONAL_B_SPLINE_CURVE((1.02147610369996,1.02311336089464,1.02428162962103))
REPRESENTATION_ITEM('')
);
#753=(
BOUNDED_CURVE()
B_SPLINE_CURVE(2,(#37575,#37576,#37577),.UNSPECIFIED.,.F.,.F.)
B_SPLINE_CURVE_WITH_KNOTS((3,3),(0.536094506482406,0.589144372850595),
 .UNSPECIFIED.)
CURVE()
GEOMETRIC_REPRESENTATION_ITEM()
RATIONAL_B_SPLINE_CURVE((1.02428162962104,1.02311336089464,1.02147610369997))
REPRESENTATION_ITEM('')
);
#754=(
BOUNDED_CURVE()
B_SPLINE_CURVE(2,(#37581,#37582,#37583),.UNSPECIFIED.,.F.,.F.)
B_SPLINE_CURVE_WITH_KNOTS((3,3),(0.21874603147716,0.271795897845345),
 .UNSPECIFIED.)
CURVE()
GEOMETRIC_REPRESENTATION_ITEM()
RATIONAL_B_SPLINE_CURVE((1.02147610369992,1.02311336089459,1.02428162962098))
REPRESENTATION_ITEM('')
);
#755=(
BOUNDED_CURVE()
B_SPLINE_CURVE(2,(#37585,#37586,#37587),.UNSPECIFIED.,.F.,.F.)
B_SPLINE_CURVE_WITH_KNOTS((3,3),(0.536094506482396,0.589144372850584),
 .UNSPECIFIED.)
CURVE()
GEOMETRIC_REPRESENTATION_ITEM()
RATIONAL_B_SPLINE_CURVE((1.024281629621,1.02311336089461,1.02147610369993))
REPRESENTATION_ITEM('')
);
#756=(
BOUNDED_CURVE()
B_SPLINE_CURVE(2,(#37591,#37592,#37593),.UNSPECIFIED.,.F.,.F.)
B_SPLINE_CURVE_WITH_KNOTS((3,3),(0.218746031477161,0.271795897845347),
 .UNSPECIFIED.)
CURVE()
GEOMETRIC_REPRESENTATION_ITEM()
RATIONAL_B_SPLINE_CURVE((1.02147610369993,1.02311336089461,1.024281629621))
REPRESENTATION_ITEM('')
);
#757=(
BOUNDED_CURVE()
B_SPLINE_CURVE(2,(#37595,#37596,#37597),.UNSPECIFIED.,.F.,.F.)
B_SPLINE_CURVE_WITH_KNOTS((3,3),(0.536094506482403,0.58914437285059),
 .UNSPECIFIED.)
CURVE()
GEOMETRIC_REPRESENTATION_ITEM()
RATIONAL_B_SPLINE_CURVE((1.02428162962099,1.0231133608946,1.02147610369993))
REPRESENTATION_ITEM('')
);
#758=(
BOUNDED_CURVE()
B_SPLINE_CURVE(2,(#37601,#37602,#37603),.UNSPECIFIED.,.F.,.F.)
B_SPLINE_CURVE_WITH_KNOTS((3,3),(0.218746031477149,0.271795897845334),
 .UNSPECIFIED.)
CURVE()
GEOMETRIC_REPRESENTATION_ITEM()
RATIONAL_B_SPLINE_CURVE((1.02147610369993,1.0231133608946,1.02428162962099))
REPRESENTATION_ITEM('')
);
#759=(
BOUNDED_CURVE()
B_SPLINE_CURVE(2,(#37605,#37606,#37607),.UNSPECIFIED.,.F.,.F.)
B_SPLINE_CURVE_WITH_KNOTS((3,3),(0.536094506482409,0.589144372850597),
 .UNSPECIFIED.)
CURVE()
GEOMETRIC_REPRESENTATION_ITEM()
RATIONAL_B_SPLINE_CURVE((1.02428162962102,1.02311336089463,1.02147610369995))
REPRESENTATION_ITEM('')
);
#760=(
BOUNDED_CURVE()
B_SPLINE_CURVE(2,(#37611,#37612,#37613),.UNSPECIFIED.,.F.,.F.)
B_SPLINE_CURVE_WITH_KNOTS((3,3),(0.218746031477158,0.271795897845347),
 .UNSPECIFIED.)
CURVE()
GEOMETRIC_REPRESENTATION_ITEM()
RATIONAL_B_SPLINE_CURVE((1.02147610370001,1.02311336089469,1.02428162962108))
REPRESENTATION_ITEM('')
);
#761=(
BOUNDED_CURVE()
B_SPLINE_CURVE(2,(#37615,#37616,#37617),.UNSPECIFIED.,.F.,.F.)
B_SPLINE_CURVE_WITH_KNOTS((3,3),(0.536094506482415,0.589144372850599),
 .UNSPECIFIED.)
CURVE()
GEOMETRIC_REPRESENTATION_ITEM()
RATIONAL_B_SPLINE_CURVE((1.02428162962096,1.02311336089458,1.0214761036999))
REPRESENTATION_ITEM('')
);
#762=(
BOUNDED_CURVE()
B_SPLINE_CURVE(2,(#37621,#37622,#37623),.UNSPECIFIED.,.F.,.F.)
B_SPLINE_CURVE_WITH_KNOTS((3,3),(0.218746031477152,0.271795897845339),
 .UNSPECIFIED.)
CURVE()
GEOMETRIC_REPRESENTATION_ITEM()
RATIONAL_B_SPLINE_CURVE((1.02147610369995,1.02311336089463,1.02428162962102))
REPRESENTATION_ITEM('')
);
#763=(
BOUNDED_CURVE()
B_SPLINE_CURVE(2,(#37625,#37626,#37627),.UNSPECIFIED.,.F.,.F.)
B_SPLINE_CURVE_WITH_KNOTS((3,3),(0.536094506482415,0.589144372850599),
 .UNSPECIFIED.)
CURVE()
GEOMETRIC_REPRESENTATION_ITEM()
RATIONAL_B_SPLINE_CURVE((1.02428162962096,1.02311336089457,1.0214761036999))
REPRESENTATION_ITEM('')
);
#764=(
BOUNDED_CURVE()
B_SPLINE_CURVE(2,(#37631,#37632,#37633),.UNSPECIFIED.,.F.,.F.)
B_SPLINE_CURVE_WITH_KNOTS((3,3),(0.218746031477149,0.271795897845338),
 .UNSPECIFIED.)
CURVE()
GEOMETRIC_REPRESENTATION_ITEM()
RATIONAL_B_SPLINE_CURVE((1.02147610370001,1.02311336089469,1.02428162962109))
REPRESENTATION_ITEM('')
);
#765=(
BOUNDED_CURVE()
B_SPLINE_CURVE(2,(#37635,#37636,#37637),.UNSPECIFIED.,.F.,.F.)
B_SPLINE_CURVE_WITH_KNOTS((3,3),(0.536094506482408,0.589144372850593),
 .UNSPECIFIED.)
CURVE()
GEOMETRIC_REPRESENTATION_ITEM()
RATIONAL_B_SPLINE_CURVE((1.02428162962098,1.02311336089459,1.02147610369992))
REPRESENTATION_ITEM('')
);
#766=(
BOUNDED_CURVE()
B_SPLINE_CURVE(2,(#37641,#37642,#37643),.UNSPECIFIED.,.F.,.F.)
B_SPLINE_CURVE_WITH_KNOTS((3,3),(0.218746031477164,0.271795897845349),
 .UNSPECIFIED.)
CURVE()
GEOMETRIC_REPRESENTATION_ITEM()
RATIONAL_B_SPLINE_CURVE((1.02147610369991,1.02311336089459,1.02428162962098))
REPRESENTATION_ITEM('')
);
#767=(
BOUNDED_CURVE()
B_SPLINE_CURVE(2,(#37645,#37646,#37647),.UNSPECIFIED.,.F.,.F.)
B_SPLINE_CURVE_WITH_KNOTS((3,3),(0.536094506482405,0.589144372850592),
 .UNSPECIFIED.)
CURVE()
GEOMETRIC_REPRESENTATION_ITEM()
RATIONAL_B_SPLINE_CURVE((1.02428162962101,1.02311336089462,1.02147610369994))
REPRESENTATION_ITEM('')
);
#768=(
BOUNDED_CURVE()
B_SPLINE_CURVE(2,(#37651,#37652,#37653),.UNSPECIFIED.,.F.,.F.)
B_SPLINE_CURVE_WITH_KNOTS((3,3),(0.218746031477147,0.271795897845335),
 .UNSPECIFIED.)
CURVE()
GEOMETRIC_REPRESENTATION_ITEM()
RATIONAL_B_SPLINE_CURVE((1.02147610369998,1.02311336089466,1.02428162962105))
REPRESENTATION_ITEM('')
);
#769=(
BOUNDED_CURVE()
B_SPLINE_CURVE(2,(#37655,#37656,#37657),.UNSPECIFIED.,.F.,.F.)
B_SPLINE_CURVE_WITH_KNOTS((3,3),(0.536094506482405,0.589144372850589),
 .UNSPECIFIED.)
CURVE()
GEOMETRIC_REPRESENTATION_ITEM()
RATIONAL_B_SPLINE_CURVE((1.02428162962092,1.02311336089453,1.02147610369986))
REPRESENTATION_ITEM('')
);
#770=(
BOUNDED_CURVE()
B_SPLINE_CURVE(2,(#37661,#37662,#37663),.UNSPECIFIED.,.F.,.F.)
B_SPLINE_CURVE_WITH_KNOTS((3,3),(0.218746031477157,0.271795897845349),
 .UNSPECIFIED.)
CURVE()
GEOMETRIC_REPRESENTATION_ITEM()
RATIONAL_B_SPLINE_CURVE((1.02147610370005,1.02311336089473,1.02428162962113))
REPRESENTATION_ITEM('')
);
#771=(
BOUNDED_CURVE()
B_SPLINE_CURVE(2,(#37665,#37666,#37667),.UNSPECIFIED.,.F.,.F.)
B_SPLINE_CURVE_WITH_KNOTS((3,3),(0.536094506482405,0.589144372850593),
 .UNSPECIFIED.)
CURVE()
GEOMETRIC_REPRESENTATION_ITEM()
RATIONAL_B_SPLINE_CURVE((1.02428162962104,1.02311336089464,1.02147610369997))
REPRESENTATION_ITEM('')
);
#772=(
BOUNDED_CURVE()
B_SPLINE_CURVE(2,(#37671,#37672,#37673),.UNSPECIFIED.,.F.,.F.)
B_SPLINE_CURVE_WITH_KNOTS((3,3),(0.218746031477155,0.271795897845342),
 .UNSPECIFIED.)
CURVE()
GEOMETRIC_REPRESENTATION_ITEM()
RATIONAL_B_SPLINE_CURVE((1.02147610369998,1.02311336089466,1.02428162962105))
REPRESENTATION_ITEM('')
);
#773=(
BOUNDED_CURVE()
B_SPLINE_CURVE(2,(#37675,#37676,#37677),.UNSPECIFIED.,.F.,.F.)
B_SPLINE_CURVE_WITH_KNOTS((3,3),(0.536094506482402,0.589144372850587),
 .UNSPECIFIED.)
CURVE()
GEOMETRIC_REPRESENTATION_ITEM()
RATIONAL_B_SPLINE_CURVE((1.02428162962096,1.02311336089458,1.0214761036999))
REPRESENTATION_ITEM('')
);
#774=(
BOUNDED_CURVE()
B_SPLINE_CURVE(2,(#37681,#37682,#37683),.UNSPECIFIED.,.F.,.F.)
B_SPLINE_CURVE_WITH_KNOTS((3,3),(0.218746031477152,0.271795897845337),
 .UNSPECIFIED.)
CURVE()
GEOMETRIC_REPRESENTATION_ITEM()
RATIONAL_B_SPLINE_CURVE((1.02147610369994,1.02311336089462,1.02428162962101))
REPRESENTATION_ITEM('')
);
#775=(
BOUNDED_CURVE()
B_SPLINE_CURVE(2,(#37685,#37686,#37687),.UNSPECIFIED.,.F.,.F.)
B_SPLINE_CURVE_WITH_KNOTS((3,3),(0.536094506482403,0.58914437285059),
 .UNSPECIFIED.)
CURVE()
GEOMETRIC_REPRESENTATION_ITEM()
RATIONAL_B_SPLINE_CURVE((1.024281629621,1.02311336089461,1.02147610369994))
REPRESENTATION_ITEM('')
);
#776=(
BOUNDED_CURVE()
B_SPLINE_CURVE(2,(#37691,#37692,#37693),.UNSPECIFIED.,.F.,.F.)
B_SPLINE_CURVE_WITH_KNOTS((3,3),(0.218746031477151,0.271795897845343),
 .UNSPECIFIED.)
CURVE()
GEOMETRIC_REPRESENTATION_ITEM()
RATIONAL_B_SPLINE_CURVE((1.02147610370007,1.02311336089475,1.02428162962115))
REPRESENTATION_ITEM('')
);
#777=(
BOUNDED_CURVE()
B_SPLINE_CURVE(2,(#37695,#37696,#37697),.UNSPECIFIED.,.F.,.F.)
B_SPLINE_CURVE_WITH_KNOTS((3,3),(0.536094506482409,0.589144372850593),
 .UNSPECIFIED.)
CURVE()
GEOMETRIC_REPRESENTATION_ITEM()
RATIONAL_B_SPLINE_CURVE((1.02428162962094,1.02311336089455,1.02147610369988))
REPRESENTATION_ITEM('')
);
#778=(
BOUNDED_CURVE()
B_SPLINE_CURVE(2,(#37701,#37702,#37703),.UNSPECIFIED.,.F.,.F.)
B_SPLINE_CURVE_WITH_KNOTS((3,3),(0.218746031477156,0.271795897845345),
 .UNSPECIFIED.)
CURVE()
GEOMETRIC_REPRESENTATION_ITEM()
RATIONAL_B_SPLINE_CURVE((1.02147610370001,1.02311336089469,1.02428162962108))
REPRESENTATION_ITEM('')
);
#779=(
BOUNDED_CURVE()
B_SPLINE_CURVE(2,(#37705,#37706,#37707),.UNSPECIFIED.,.F.,.F.)
B_SPLINE_CURVE_WITH_KNOTS((3,3),(0.536094506482414,0.589144372850603),
 .UNSPECIFIED.)
CURVE()
GEOMETRIC_REPRESENTATION_ITEM()
RATIONAL_B_SPLINE_CURVE((1.02428162962107,1.02311336089467,1.02147610369999))
REPRESENTATION_ITEM('')
);
#780=(
BOUNDED_CURVE()
B_SPLINE_CURVE(2,(#37711,#37712,#37713),.UNSPECIFIED.,.F.,.F.)
B_SPLINE_CURVE_WITH_KNOTS((3,3),(0.218746031477163,0.271795897845352),
 .UNSPECIFIED.)
CURVE()
GEOMETRIC_REPRESENTATION_ITEM()
RATIONAL_B_SPLINE_CURVE((1.02147610369999,1.02311336089467,1.02428162962106))
REPRESENTATION_ITEM('')
);
#781=(
BOUNDED_CURVE()
B_SPLINE_CURVE(2,(#37715,#37716,#37717),.UNSPECIFIED.,.F.,.F.)
B_SPLINE_CURVE_WITH_KNOTS((3,3),(0.536094506482405,0.58914437285059),
 .UNSPECIFIED.)
CURVE()
GEOMETRIC_REPRESENTATION_ITEM()
RATIONAL_B_SPLINE_CURVE((1.02428162962097,1.02311336089458,1.02147610369991))
REPRESENTATION_ITEM('')
);
#782=(
BOUNDED_CURVE()
B_SPLINE_CURVE(2,(#37721,#37722,#37723),.UNSPECIFIED.,.F.,.F.)
B_SPLINE_CURVE_WITH_KNOTS((3,3),(0.218746031477157,0.27179589784534),
 .UNSPECIFIED.)
CURVE()
GEOMETRIC_REPRESENTATION_ITEM()
RATIONAL_B_SPLINE_CURVE((1.02147610369987,1.02311336089454,1.02428162962093))
REPRESENTATION_ITEM('')
);
#783=(
BOUNDED_CURVE()
B_SPLINE_CURVE(2,(#37725,#37726,#37727),.UNSPECIFIED.,.F.,.F.)
B_SPLINE_CURVE_WITH_KNOTS((3,3),(0.536094506482407,0.589144372850599),
 .UNSPECIFIED.)
CURVE()
GEOMETRIC_REPRESENTATION_ITEM()
RATIONAL_B_SPLINE_CURVE((1.02428162962112,1.02311336089472,1.02147610370004))
REPRESENTATION_ITEM('')
);
#784=(
BOUNDED_CURVE()
B_SPLINE_CURVE(2,(#37731,#37732,#37733),.UNSPECIFIED.,.F.,.F.)
B_SPLINE_CURVE_WITH_KNOTS((3,3),(-0.271795897845351,-0.270098893534586),
 .UNSPECIFIED.)
CURVE()
GEOMETRIC_REPRESENTATION_ITEM()
RATIONAL_B_SPLINE_CURVE((1.02428162962102,1.02424425804592,1.02420640656119))
REPRESENTATION_ITEM('')
);
#785=(
BOUNDED_CURVE()
B_SPLINE_CURVE(2,(#37738,#37739,#37740),.UNSPECIFIED.,.F.,.F.)
B_SPLINE_CURVE_WITH_KNOTS((3,3),(-0.270098893534586,-0.218746031477164),
 .UNSPECIFIED.)
CURVE()
GEOMETRIC_REPRESENTATION_ITEM()
RATIONAL_B_SPLINE_CURVE((1.02420640656119,1.02306098691695,1.02147610369995))
REPRESENTATION_ITEM('')
);
#786=(
BOUNDED_CURVE()
B_SPLINE_CURVE(2,(#37742,#37743,#37744),.UNSPECIFIED.,.F.,.F.)
B_SPLINE_CURVE_WITH_KNOTS((3,3),(0.536094506482404,0.589144372850591),
 .UNSPECIFIED.)
CURVE()
GEOMETRIC_REPRESENTATION_ITEM()
RATIONAL_B_SPLINE_CURVE((1.02428162962101,1.02311336089462,1.02147610369994))
REPRESENTATION_ITEM('')
);
#787=(
BOUNDED_CURVE()
B_SPLINE_CURVE(2,(#37748,#37749,#37750),.UNSPECIFIED.,.F.,.F.)
B_SPLINE_CURVE_WITH_KNOTS((3,3),(0.218746031477165,0.271795897845351),
 .UNSPECIFIED.)
CURVE()
GEOMETRIC_REPRESENTATION_ITEM()
RATIONAL_B_SPLINE_CURVE((1.02147610369995,1.02311336089462,1.02428162962101))
REPRESENTATION_ITEM('')
);
#788=(
BOUNDED_CURVE()
B_SPLINE_CURVE(2,(#37752,#37753,#37754),.UNSPECIFIED.,.F.,.F.)
B_SPLINE_CURVE_WITH_KNOTS((3,3),(0.536094506482406,0.589144372850597),
 .UNSPECIFIED.)
CURVE()
GEOMETRIC_REPRESENTATION_ITEM()
RATIONAL_B_SPLINE_CURVE((1.02428162962109,1.02311336089469,1.02147610370001))
REPRESENTATION_ITEM('')
);
#789=(
BOUNDED_CURVE()
B_SPLINE_CURVE(2,(#37758,#37759,#37760),.UNSPECIFIED.,.F.,.F.)
B_SPLINE_CURVE_WITH_KNOTS((3,3),(0.218746031477132,0.271795897845324),
 .UNSPECIFIED.)
CURVE()
GEOMETRIC_REPRESENTATION_ITEM()
RATIONAL_B_SPLINE_CURVE((1.02147610370008,1.02311336089477,1.02428162962117))
REPRESENTATION_ITEM('')
);
#790=(
BOUNDED_CURVE()
B_SPLINE_CURVE(2,(#37762,#37763,#37764),.UNSPECIFIED.,.F.,.F.)
B_SPLINE_CURVE_WITH_KNOTS((3,3),(0.536094506482402,0.589144372850584),
 .UNSPECIFIED.)
CURVE()
GEOMETRIC_REPRESENTATION_ITEM()
RATIONAL_B_SPLINE_CURVE((1.02428162962088,1.0231133608945,1.02147610369983))
REPRESENTATION_ITEM('')
);
#791=(
BOUNDED_CURVE()
B_SPLINE_CURVE(2,(#37768,#37769,#37770),.UNSPECIFIED.,.F.,.F.)
B_SPLINE_CURVE_WITH_KNOTS((3,3),(0.218746031477161,0.271795897845343),
 .UNSPECIFIED.)
CURVE()
GEOMETRIC_REPRESENTATION_ITEM()
RATIONAL_B_SPLINE_CURVE((1.02147610369988,1.02311336089455,1.02428162962093))
REPRESENTATION_ITEM('')
);
#792=(
BOUNDED_CURVE()
B_SPLINE_CURVE(2,(#37772,#37773,#37774),.UNSPECIFIED.,.F.,.F.)
B_SPLINE_CURVE_WITH_KNOTS((3,3),(0.536094506482405,0.589144372850588),
 .UNSPECIFIED.)
CURVE()
GEOMETRIC_REPRESENTATION_ITEM()
RATIONAL_B_SPLINE_CURVE((1.02428162962095,1.02311336089456,1.02147610369989))
REPRESENTATION_ITEM('')
);
#793=(
BOUNDED_CURVE()
B_SPLINE_CURVE(2,(#37778,#37779,#37780),.UNSPECIFIED.,.F.,.F.)
B_SPLINE_CURVE_WITH_KNOTS((3,3),(0.218746031477168,0.271795897845349),
 .UNSPECIFIED.)
CURVE()
GEOMETRIC_REPRESENTATION_ITEM()
RATIONAL_B_SPLINE_CURVE((1.02147610369985,1.02311336089452,1.0242816296209))
REPRESENTATION_ITEM('')
);
#794=(
BOUNDED_CURVE()
B_SPLINE_CURVE(2,(#37782,#37783,#37784),.UNSPECIFIED.,.F.,.F.)
B_SPLINE_CURVE_WITH_KNOTS((3,3),(0.536094506482408,0.589144372850595),
 .UNSPECIFIED.)
CURVE()
GEOMETRIC_REPRESENTATION_ITEM()
RATIONAL_B_SPLINE_CURVE((1.024281629621,1.02311336089461,1.02147610369993))
REPRESENTATION_ITEM('')
);
#795=(
BOUNDED_CURVE()
B_SPLINE_CURVE(2,(#37788,#37789,#37790),.UNSPECIFIED.,.F.,.F.)
B_SPLINE_CURVE_WITH_KNOTS((3,3),(0.218746031477171,0.271795897845352),
 .UNSPECIFIED.)
CURVE()
GEOMETRIC_REPRESENTATION_ITEM()
RATIONAL_B_SPLINE_CURVE((1.02147610369985,1.02311336089452,1.0242816296209))
REPRESENTATION_ITEM('')
);
#796=(
BOUNDED_CURVE()
B_SPLINE_CURVE(2,(#37792,#37793,#37794),.UNSPECIFIED.,.F.,.F.)
B_SPLINE_CURVE_WITH_KNOTS((3,3),(0.536094506482397,0.589144372850578),
 .UNSPECIFIED.)
CURVE()
GEOMETRIC_REPRESENTATION_ITEM()
RATIONAL_B_SPLINE_CURVE((1.02428162962088,1.02311336089449,1.02147610369983))
REPRESENTATION_ITEM('')
);
#797=(
BOUNDED_CURVE()
B_SPLINE_CURVE(2,(#37798,#37799,#37800),.UNSPECIFIED.,.F.,.F.)
B_SPLINE_CURVE_WITH_KNOTS((3,3),(0.218746031477161,0.271795897845346),
 .UNSPECIFIED.)
CURVE()
GEOMETRIC_REPRESENTATION_ITEM()
RATIONAL_B_SPLINE_CURVE((1.02147610369991,1.02311336089458,1.02428162962097))
REPRESENTATION_ITEM('')
);
#798=(
BOUNDED_CURVE()
B_SPLINE_CURVE(2,(#37802,#37803,#37804),.UNSPECIFIED.,.F.,.F.)
B_SPLINE_CURVE_WITH_KNOTS((3,3),(0.536094506482397,0.589144372850583),
 .UNSPECIFIED.)
CURVE()
GEOMETRIC_REPRESENTATION_ITEM()
RATIONAL_B_SPLINE_CURVE((1.02428162962098,1.02311336089459,1.02147610369992))
REPRESENTATION_ITEM('')
);
#799=(
BOUNDED_CURVE()
B_SPLINE_CURVE(2,(#37808,#37809,#37810),.UNSPECIFIED.,.F.,.F.)
B_SPLINE_CURVE_WITH_KNOTS((3,3),(0.218746031477178,0.271795897845362),
 .UNSPECIFIED.)
CURVE()
GEOMETRIC_REPRESENTATION_ITEM()
RATIONAL_B_SPLINE_CURVE((1.02147610369987,1.02311336089454,1.02428162962093))
REPRESENTATION_ITEM('')
);
#800=(
BOUNDED_CURVE()
B_SPLINE_CURVE(2,(#37812,#37813,#37814),.UNSPECIFIED.,.F.,.F.)
B_SPLINE_CURVE_WITH_KNOTS((3,3),(0.536094506482401,0.589144372850588),
 .UNSPECIFIED.)
CURVE()
GEOMETRIC_REPRESENTATION_ITEM()
RATIONAL_B_SPLINE_CURVE((1.02428162962099,1.0231133608946,1.02147610369993))
REPRESENTATION_ITEM('')
);
#801=(
BOUNDED_CURVE()
B_SPLINE_CURVE(2,(#37818,#37819,#37820),.UNSPECIFIED.,.F.,.F.)
B_SPLINE_CURVE_WITH_KNOTS((3,3),(0.218746031477169,0.271795897845355),
 .UNSPECIFIED.)
CURVE()
GEOMETRIC_REPRESENTATION_ITEM()
RATIONAL_B_SPLINE_CURVE((1.02147610369993,1.02311336089461,1.024281629621))
REPRESENTATION_ITEM('')
);
#802=(
BOUNDED_CURVE()
B_SPLINE_CURVE(2,(#37822,#37823,#37824),.UNSPECIFIED.,.F.,.F.)
B_SPLINE_CURVE_WITH_KNOTS((3,3),(0.536094506482416,0.589144372850602),
 .UNSPECIFIED.)
CURVE()
GEOMETRIC_REPRESENTATION_ITEM()
RATIONAL_B_SPLINE_CURVE((1.02428162962103,1.02311336089464,1.02147610369996))
REPRESENTATION_ITEM('')
);
#803=(
BOUNDED_CURVE()
B_SPLINE_CURVE(2,(#37828,#37829,#37830),.UNSPECIFIED.,.F.,.F.)
B_SPLINE_CURVE_WITH_KNOTS((3,3),(0.218746031477151,0.271795897845338),
 .UNSPECIFIED.)
CURVE()
GEOMETRIC_REPRESENTATION_ITEM()
RATIONAL_B_SPLINE_CURVE((1.02147610369997,1.02311336089465,1.02428162962104))
REPRESENTATION_ITEM('')
);
#804=(
BOUNDED_CURVE()
B_SPLINE_CURVE(2,(#37832,#37833,#37834),.UNSPECIFIED.,.F.,.F.)
B_SPLINE_CURVE_WITH_KNOTS((3,3),(0.536094506482404,0.589144372850587),
 .UNSPECIFIED.)
CURVE()
GEOMETRIC_REPRESENTATION_ITEM()
RATIONAL_B_SPLINE_CURVE((1.02428162962093,1.02311336089454,1.02147610369987))
REPRESENTATION_ITEM('')
);
#805=(
BOUNDED_CURVE()
B_SPLINE_CURVE(2,(#37838,#37839,#37840),.UNSPECIFIED.,.F.,.F.)
B_SPLINE_CURVE_WITH_KNOTS((3,3),(0.21874603147716,0.271795897845347),
 .UNSPECIFIED.)
CURVE()
GEOMETRIC_REPRESENTATION_ITEM()
RATIONAL_B_SPLINE_CURVE((1.02147610369994,1.02311336089462,1.02428162962101))
REPRESENTATION_ITEM('')
);
#806=(
BOUNDED_CURVE()
B_SPLINE_CURVE(2,(#37842,#37843,#37844),.UNSPECIFIED.,.F.,.F.)
B_SPLINE_CURVE_WITH_KNOTS((3,3),(0.536094506482402,0.589144372850585),
 .UNSPECIFIED.)
CURVE()
GEOMETRIC_REPRESENTATION_ITEM()
RATIONAL_B_SPLINE_CURVE((1.02428162962091,1.02311336089452,1.02147610369985))
REPRESENTATION_ITEM('')
);
#807=(
BOUNDED_CURVE()
B_SPLINE_CURVE(2,(#37848,#37849,#37850),.UNSPECIFIED.,.F.,.F.)
B_SPLINE_CURVE_WITH_KNOTS((3,3),(0.218746031477168,0.271795897845356),
 .UNSPECIFIED.)
CURVE()
GEOMETRIC_REPRESENTATION_ITEM()
RATIONAL_B_SPLINE_CURVE((1.02147610369995,1.02311336089462,1.02428162962101))
REPRESENTATION_ITEM('')
);
#808=(
BOUNDED_CURVE()
B_SPLINE_CURVE(2,(#37852,#37853,#37854),.UNSPECIFIED.,.F.,.F.)
B_SPLINE_CURVE_WITH_KNOTS((3,3),(0.536094506482419,0.589144372850602),
 .UNSPECIFIED.)
CURVE()
GEOMETRIC_REPRESENTATION_ITEM()
RATIONAL_B_SPLINE_CURVE((1.02428162962094,1.02311336089456,1.02147610369988))
REPRESENTATION_ITEM('')
);
#809=(
BOUNDED_CURVE()
B_SPLINE_CURVE(2,(#37858,#37859,#37860),.UNSPECIFIED.,.F.,.F.)
B_SPLINE_CURVE_WITH_KNOTS((3,3),(0.218746031477172,0.271795897845351),
 .UNSPECIFIED.)
CURVE()
GEOMETRIC_REPRESENTATION_ITEM()
RATIONAL_B_SPLINE_CURVE((1.02147610369981,1.02311336089447,1.02428162962086))
REPRESENTATION_ITEM('')
);
#810=(
BOUNDED_CURVE()
B_SPLINE_CURVE(2,(#37862,#37863,#37864),.UNSPECIFIED.,.F.,.F.)
B_SPLINE_CURVE_WITH_KNOTS((3,3),(0.536094506482413,0.589144372850597),
 .UNSPECIFIED.)
CURVE()
GEOMETRIC_REPRESENTATION_ITEM()
RATIONAL_B_SPLINE_CURVE((1.02428162962095,1.02311336089456,1.02147610369989))
REPRESENTATION_ITEM('')
);
#811=(
BOUNDED_CURVE()
B_SPLINE_CURVE(2,(#37868,#37869,#37870),.UNSPECIFIED.,.F.,.F.)
B_SPLINE_CURVE_WITH_KNOTS((3,3),(0.218746031477175,0.271795897845363),
 .UNSPECIFIED.)
CURVE()
GEOMETRIC_REPRESENTATION_ITEM()
RATIONAL_B_SPLINE_CURVE((1.02147610369996,1.02311336089463,1.02428162962103))
REPRESENTATION_ITEM('')
);
#812=(
BOUNDED_CURVE()
B_SPLINE_CURVE(2,(#37872,#37873,#37874),.UNSPECIFIED.,.F.,.F.)
B_SPLINE_CURVE_WITH_KNOTS((3,3),(0.536094506482418,0.589144372850602),
 .UNSPECIFIED.)
CURVE()
GEOMETRIC_REPRESENTATION_ITEM()
RATIONAL_B_SPLINE_CURVE((1.02428162962098,1.02311336089459,1.02147610369991))
REPRESENTATION_ITEM('')
);
#813=(
BOUNDED_CURVE()
B_SPLINE_CURVE(2,(#37878,#37879,#37880),.UNSPECIFIED.,.F.,.F.)
B_SPLINE_CURVE_WITH_KNOTS((3,3),(0.21874603147716,0.271795897845347),
 .UNSPECIFIED.)
CURVE()
GEOMETRIC_REPRESENTATION_ITEM()
RATIONAL_B_SPLINE_CURVE((1.02147610369995,1.02311336089463,1.02428162962102))
REPRESENTATION_ITEM('')
);
#814=(
BOUNDED_CURVE()
B_SPLINE_CURVE(2,(#37882,#37883,#37884),.UNSPECIFIED.,.F.,.F.)
B_SPLINE_CURVE_WITH_KNOTS((3,3),(0.536094506482396,0.589144372850583),
 .UNSPECIFIED.)
CURVE()
GEOMETRIC_REPRESENTATION_ITEM()
RATIONAL_B_SPLINE_CURVE((1.02428162962099,1.0231133608946,1.02147610369992))
REPRESENTATION_ITEM('')
);
#815=(
BOUNDED_CURVE()
B_SPLINE_CURVE(2,(#37888,#37889,#37890),.UNSPECIFIED.,.F.,.F.)
B_SPLINE_CURVE_WITH_KNOTS((3,3),(0.218746031477158,0.271795897845343),
 .UNSPECIFIED.)
CURVE()
GEOMETRIC_REPRESENTATION_ITEM()
RATIONAL_B_SPLINE_CURVE((1.02147610369992,1.02311336089459,1.02428162962098))
REPRESENTATION_ITEM('')
);
#816=(
BOUNDED_CURVE()
B_SPLINE_CURVE(2,(#37892,#37893,#37894),.UNSPECIFIED.,.F.,.F.)
B_SPLINE_CURVE_WITH_KNOTS((3,3),(0.536094506482406,0.589144372850593),
 .UNSPECIFIED.)
CURVE()
GEOMETRIC_REPRESENTATION_ITEM()
RATIONAL_B_SPLINE_CURVE((1.02428162962099,1.0231133608946,1.02147610369993))
REPRESENTATION_ITEM('')
);
#817=(
BOUNDED_CURVE()
B_SPLINE_CURVE(2,(#37898,#37899,#37900),.UNSPECIFIED.,.F.,.F.)
B_SPLINE_CURVE_WITH_KNOTS((3,3),(0.218746031477158,0.271795897845344),
 .UNSPECIFIED.)
CURVE()
GEOMETRIC_REPRESENTATION_ITEM()
RATIONAL_B_SPLINE_CURVE((1.02147610369995,1.02311336089462,1.02428162962101))
REPRESENTATION_ITEM('')
);
#818=(
BOUNDED_CURVE()
B_SPLINE_CURVE(2,(#37902,#37903,#37904),.UNSPECIFIED.,.F.,.F.)
B_SPLINE_CURVE_WITH_KNOTS((3,3),(0.536094506482404,0.589144372850588),
 .UNSPECIFIED.)
CURVE()
GEOMETRIC_REPRESENTATION_ITEM()
RATIONAL_B_SPLINE_CURVE((1.02428162962094,1.02311336089456,1.02147610369989))
REPRESENTATION_ITEM('')
);
#819=(
BOUNDED_CURVE()
B_SPLINE_CURVE(2,(#37908,#37909,#37910),.UNSPECIFIED.,.F.,.F.)
B_SPLINE_CURVE_WITH_KNOTS((3,3),(0.218746031477163,0.271795897845347),
 .UNSPECIFIED.)
CURVE()
GEOMETRIC_REPRESENTATION_ITEM()
RATIONAL_B_SPLINE_CURVE((1.0214761036999,1.02311336089458,1.02428162962097))
REPRESENTATION_ITEM('')
);
#820=(
BOUNDED_CURVE()
B_SPLINE_CURVE(2,(#37912,#37913,#37914),.UNSPECIFIED.,.F.,.F.)
B_SPLINE_CURVE_WITH_KNOTS((3,3),(0.536094506482397,0.589144372850583),
 .UNSPECIFIED.)
CURVE()
GEOMETRIC_REPRESENTATION_ITEM()
RATIONAL_B_SPLINE_CURVE((1.02428162962099,1.0231133608946,1.02147610369992))
REPRESENTATION_ITEM('')
);
#821=(
BOUNDED_CURVE()
B_SPLINE_CURVE(2,(#37918,#37919,#37920),.UNSPECIFIED.,.F.,.F.)
B_SPLINE_CURVE_WITH_KNOTS((3,3),(0.218746031477164,0.271795897845345),
 .UNSPECIFIED.)
CURVE()
GEOMETRIC_REPRESENTATION_ITEM()
RATIONAL_B_SPLINE_CURVE((1.02147610369985,1.02311336089451,1.0242816296209))
REPRESENTATION_ITEM('')
);
#822=(
BOUNDED_CURVE()
B_SPLINE_CURVE(2,(#37922,#37923,#37924),.UNSPECIFIED.,.F.,.F.)
B_SPLINE_CURVE_WITH_KNOTS((3,3),(0.536094506482409,0.589144372850595),
 .UNSPECIFIED.)
CURVE()
GEOMETRIC_REPRESENTATION_ITEM()
RATIONAL_B_SPLINE_CURVE((1.02428162962099,1.0231133608946,1.02147610369992))
REPRESENTATION_ITEM('')
);
#823=(
BOUNDED_CURVE()
B_SPLINE_CURVE(2,(#37928,#37929,#37930),.UNSPECIFIED.,.F.,.F.)
B_SPLINE_CURVE_WITH_KNOTS((3,3),(0.218746031477171,0.271795897845354),
 .UNSPECIFIED.)
CURVE()
GEOMETRIC_REPRESENTATION_ITEM()
RATIONAL_B_SPLINE_CURVE((1.02147610369987,1.02311336089454,1.02428162962093))
REPRESENTATION_ITEM('')
);
#824=(
BOUNDED_CURVE()
B_SPLINE_CURVE(2,(#37932,#37933,#37934),.UNSPECIFIED.,.F.,.F.)
B_SPLINE_CURVE_WITH_KNOTS((3,3),(0.536094506482407,0.589144372850591),
 .UNSPECIFIED.)
CURVE()
GEOMETRIC_REPRESENTATION_ITEM()
RATIONAL_B_SPLINE_CURVE((1.02428162962096,1.02311336089457,1.0214761036999))
REPRESENTATION_ITEM('')
);
#825=(
BOUNDED_CURVE()
B_SPLINE_CURVE(2,(#37938,#37939,#37940),.UNSPECIFIED.,.F.,.F.)
B_SPLINE_CURVE_WITH_KNOTS((3,3),(0.218746031477165,0.271795897845349),
 .UNSPECIFIED.)
CURVE()
GEOMETRIC_REPRESENTATION_ITEM()
RATIONAL_B_SPLINE_CURVE((1.0214761036999,1.02311336089457,1.02428162962096))
REPRESENTATION_ITEM('')
);
#826=(
BOUNDED_CURVE()
B_SPLINE_CURVE(2,(#37942,#37943,#37944),.UNSPECIFIED.,.F.,.F.)
B_SPLINE_CURVE_WITH_KNOTS((3,3),(0.53609450648241,0.589144372850595),
 .UNSPECIFIED.)
CURVE()
GEOMETRIC_REPRESENTATION_ITEM()
RATIONAL_B_SPLINE_CURVE((1.02428162962096,1.02311336089458,1.0214761036999))
REPRESENTATION_ITEM('')
);
#827=(
BOUNDED_CURVE()
B_SPLINE_CURVE(2,(#37948,#37949,#37950),.UNSPECIFIED.,.F.,.F.)
B_SPLINE_CURVE_WITH_KNOTS((3,3),(0.218746031477166,0.271795897845348),
 .UNSPECIFIED.)
CURVE()
GEOMETRIC_REPRESENTATION_ITEM()
RATIONAL_B_SPLINE_CURVE((1.02147610369988,1.02311336089455,1.02428162962094))
REPRESENTATION_ITEM('')
);
#828=(
BOUNDED_CURVE()
B_SPLINE_CURVE(2,(#37952,#37953,#37954),.UNSPECIFIED.,.F.,.F.)
B_SPLINE_CURVE_WITH_KNOTS((3,3),(0.53609450648241,0.589144372850593),
 .UNSPECIFIED.)
CURVE()
GEOMETRIC_REPRESENTATION_ITEM()
RATIONAL_B_SPLINE_CURVE((1.02428162962095,1.02311336089456,1.02147610369989))
REPRESENTATION_ITEM('')
);
#829=(
BOUNDED_CURVE()
B_SPLINE_CURVE(2,(#37958,#37959,#37960),.UNSPECIFIED.,.F.,.F.)
B_SPLINE_CURVE_WITH_KNOTS((3,3),(0.21874603147716,0.271795897845347),
 .UNSPECIFIED.)
CURVE()
GEOMETRIC_REPRESENTATION_ITEM()
RATIONAL_B_SPLINE_CURVE((1.02147610369996,1.02311336089463,1.02428162962102))
REPRESENTATION_ITEM('')
);
#830=(
BOUNDED_CURVE()
B_SPLINE_CURVE(2,(#37962,#37963,#37964),.UNSPECIFIED.,.F.,.F.)
B_SPLINE_CURVE_WITH_KNOTS((3,3),(0.53609450648241,0.589144372850594),
 .UNSPECIFIED.)
CURVE()
GEOMETRIC_REPRESENTATION_ITEM()
RATIONAL_B_SPLINE_CURVE((1.02428162962095,1.02311336089456,1.02147610369989))
REPRESENTATION_ITEM('')
);
#831=(
BOUNDED_CURVE()
B_SPLINE_CURVE(2,(#37968,#37969,#37970),.UNSPECIFIED.,.F.,.F.)
B_SPLINE_CURVE_WITH_KNOTS((3,3),(0.218746031477162,0.271795897845348),
 .UNSPECIFIED.)
CURVE()
GEOMETRIC_REPRESENTATION_ITEM()
RATIONAL_B_SPLINE_CURVE((1.02147610369995,1.02311336089463,1.02428162962102))
REPRESENTATION_ITEM('')
);
#832=(
BOUNDED_CURVE()
B_SPLINE_CURVE(2,(#37972,#37973,#37974),.UNSPECIFIED.,.F.,.F.)
B_SPLINE_CURVE_WITH_KNOTS((3,3),(0.536094506482406,0.589144372850593),
 .UNSPECIFIED.)
CURVE()
GEOMETRIC_REPRESENTATION_ITEM()
RATIONAL_B_SPLINE_CURVE((1.024281629621,1.02311336089461,1.02147610369993))
REPRESENTATION_ITEM('')
);
#833=(
BOUNDED_CURVE()
B_SPLINE_CURVE(2,(#37978,#37979,#37980),.UNSPECIFIED.,.F.,.F.)
B_SPLINE_CURVE_WITH_KNOTS((3,3),(0.218746031477166,0.271795897845352),
 .UNSPECIFIED.)
CURVE()
GEOMETRIC_REPRESENTATION_ITEM()
RATIONAL_B_SPLINE_CURVE((1.02147610369994,1.02311336089462,1.02428162962101))
REPRESENTATION_ITEM('')
);
#834=(
BOUNDED_CURVE()
B_SPLINE_CURVE(2,(#37982,#37983,#37984),.UNSPECIFIED.,.F.,.F.)
B_SPLINE_CURVE_WITH_KNOTS((3,3),(0.536094506482414,0.589144372850599),
 .UNSPECIFIED.)
CURVE()
GEOMETRIC_REPRESENTATION_ITEM()
RATIONAL_B_SPLINE_CURVE((1.02428162962095,1.02311336089456,1.02147610369989))
REPRESENTATION_ITEM('')
);
#835=(
BOUNDED_CURVE()
B_SPLINE_CURVE(2,(#37988,#37989,#37990),.UNSPECIFIED.,.F.,.F.)
B_SPLINE_CURVE_WITH_KNOTS((3,3),(0.218746031477169,0.271795897845355),
 .UNSPECIFIED.)
CURVE()
GEOMETRIC_REPRESENTATION_ITEM()
RATIONAL_B_SPLINE_CURVE((1.02147610369993,1.0231133608946,1.02428162962099))
REPRESENTATION_ITEM('')
);
#836=(
BOUNDED_CURVE()
B_SPLINE_CURVE(2,(#37992,#37993,#37994),.UNSPECIFIED.,.F.,.F.)
B_SPLINE_CURVE_WITH_KNOTS((3,3),(0.536094506482414,0.589144372850597),
 .UNSPECIFIED.)
CURVE()
GEOMETRIC_REPRESENTATION_ITEM()
RATIONAL_B_SPLINE_CURVE((1.02428162962095,1.02311336089457,1.02147610369989))
REPRESENTATION_ITEM('')
);
#837=(
BOUNDED_CURVE()
B_SPLINE_CURVE(2,(#37998,#37999,#38000),.UNSPECIFIED.,.F.,.F.)
B_SPLINE_CURVE_WITH_KNOTS((3,3),(0.218746031477173,0.271795897845359),
 .UNSPECIFIED.)
CURVE()
GEOMETRIC_REPRESENTATION_ITEM()
RATIONAL_B_SPLINE_CURVE((1.02147610369992,1.02311336089459,1.02428162962098))
REPRESENTATION_ITEM('')
);
#838=(
BOUNDED_CURVE()
B_SPLINE_CURVE(2,(#38002,#38003,#38004),.UNSPECIFIED.,.F.,.F.)
B_SPLINE_CURVE_WITH_KNOTS((3,3),(0.536094506482406,0.589144372850592),
 .UNSPECIFIED.)
CURVE()
GEOMETRIC_REPRESENTATION_ITEM()
RATIONAL_B_SPLINE_CURVE((1.02428162962098,1.02311336089459,1.02147610369992))
REPRESENTATION_ITEM('')
);
#839=(
BOUNDED_CURVE()
B_SPLINE_CURVE(2,(#38008,#38009,#38010),.UNSPECIFIED.,.F.,.F.)
B_SPLINE_CURVE_WITH_KNOTS((3,3),(0.218746031477167,0.271795897845351),
 .UNSPECIFIED.)
CURVE()
GEOMETRIC_REPRESENTATION_ITEM()
RATIONAL_B_SPLINE_CURVE((1.02147610369989,1.02311336089456,1.02428162962095))
REPRESENTATION_ITEM('')
);
#840=(
BOUNDED_CURVE()
B_SPLINE_CURVE(2,(#38012,#38013,#38014),.UNSPECIFIED.,.F.,.F.)
B_SPLINE_CURVE_WITH_KNOTS((3,3),(0.536094506482407,0.589144372850592),
 .UNSPECIFIED.)
CURVE()
GEOMETRIC_REPRESENTATION_ITEM()
RATIONAL_B_SPLINE_CURVE((1.02428162962097,1.02311336089458,1.02147610369991))
REPRESENTATION_ITEM('')
);
#841=(
BOUNDED_CURVE()
B_SPLINE_CURVE(2,(#38018,#38019,#38020),.UNSPECIFIED.,.F.,.F.)
B_SPLINE_CURVE_WITH_KNOTS((3,3),(0.218746031477175,0.271795897845359),
 .UNSPECIFIED.)
CURVE()
GEOMETRIC_REPRESENTATION_ITEM()
RATIONAL_B_SPLINE_CURVE((1.02147610369989,1.02311336089456,1.02428162962095))
REPRESENTATION_ITEM('')
);
#842=(
BOUNDED_CURVE()
B_SPLINE_CURVE(2,(#38022,#38023,#38024),.UNSPECIFIED.,.F.,.F.)
B_SPLINE_CURVE_WITH_KNOTS((3,3),(0.536094506482402,0.589144372850588),
 .UNSPECIFIED.)
CURVE()
GEOMETRIC_REPRESENTATION_ITEM()
RATIONAL_B_SPLINE_CURVE((1.02428162962098,1.02311336089459,1.02147610369991))
REPRESENTATION_ITEM('')
);
#843=(
BOUNDED_CURVE()
B_SPLINE_CURVE(2,(#38028,#38029,#38030),.UNSPECIFIED.,.F.,.F.)
B_SPLINE_CURVE_WITH_KNOTS((3,3),(0.218746031477175,0.271795897845355),
 .UNSPECIFIED.)
CURVE()
GEOMETRIC_REPRESENTATION_ITEM()
RATIONAL_B_SPLINE_CURVE((1.02147610369982,1.02311336089449,1.02428162962087))
REPRESENTATION_ITEM('')
);
#844=(
BOUNDED_CURVE()
B_SPLINE_CURVE(2,(#38032,#38033,#38034),.UNSPECIFIED.,.F.,.F.)
B_SPLINE_CURVE_WITH_KNOTS((3,3),(0.536094506482407,0.589144372850592),
 .UNSPECIFIED.)
CURVE()
GEOMETRIC_REPRESENTATION_ITEM()
RATIONAL_B_SPLINE_CURVE((1.02428162962096,1.02311336089457,1.0214761036999))
REPRESENTATION_ITEM('')
);
#845=(
BOUNDED_CURVE()
B_SPLINE_CURVE(2,(#38038,#38039,#38040),.UNSPECIFIED.,.F.,.F.)
B_SPLINE_CURVE_WITH_KNOTS((3,3),(0.21874603147717,0.271795897845352),
 .UNSPECIFIED.)
CURVE()
GEOMETRIC_REPRESENTATION_ITEM()
RATIONAL_B_SPLINE_CURVE((1.02147610369985,1.02311336089452,1.02428162962091))
REPRESENTATION_ITEM('')
);
#846=(
BOUNDED_CURVE()
B_SPLINE_CURVE(2,(#38042,#38043,#38044),.UNSPECIFIED.,.F.,.F.)
B_SPLINE_CURVE_WITH_KNOTS((3,3),(0.536094506482403,0.589144372850591),
 .UNSPECIFIED.)
CURVE()
GEOMETRIC_REPRESENTATION_ITEM()
RATIONAL_B_SPLINE_CURVE((1.02428162962102,1.02311336089463,1.02147610369996))
REPRESENTATION_ITEM('')
);
#847=(
BOUNDED_CURVE()
B_SPLINE_CURVE(2,(#38048,#38049,#38050),.UNSPECIFIED.,.F.,.F.)
B_SPLINE_CURVE_WITH_KNOTS((3,3),(0.218746031477164,0.271795897845349),
 .UNSPECIFIED.)
CURVE()
GEOMETRIC_REPRESENTATION_ITEM()
RATIONAL_B_SPLINE_CURVE((1.02147610369991,1.02311336089459,1.02428162962097))
REPRESENTATION_ITEM('')
);
#848=(
BOUNDED_CURVE()
B_SPLINE_CURVE(2,(#38052,#38053,#38054),.UNSPECIFIED.,.F.,.F.)
B_SPLINE_CURVE_WITH_KNOTS((3,3),(0.536094506482412,0.589144372850596),
 .UNSPECIFIED.)
CURVE()
GEOMETRIC_REPRESENTATION_ITEM()
RATIONAL_B_SPLINE_CURVE((1.02428162962096,1.02311336089457,1.0214761036999))
REPRESENTATION_ITEM('')
);
#849=(
BOUNDED_CURVE()
B_SPLINE_CURVE(2,(#38058,#38059,#38060),.UNSPECIFIED.,.F.,.F.)
B_SPLINE_CURVE_WITH_KNOTS((3,3),(0.218746031477168,0.27179589784535),
 .UNSPECIFIED.)
CURVE()
GEOMETRIC_REPRESENTATION_ITEM()
RATIONAL_B_SPLINE_CURVE((1.02147610369985,1.02311336089452,1.0242816296209))
REPRESENTATION_ITEM('')
);
#850=(
BOUNDED_CURVE()
B_SPLINE_CURVE(2,(#38062,#38063,#38064),.UNSPECIFIED.,.F.,.F.)
B_SPLINE_CURVE_WITH_KNOTS((3,3),(0.536094506482416,0.589144372850602),
 .UNSPECIFIED.)
CURVE()
GEOMETRIC_REPRESENTATION_ITEM()
RATIONAL_B_SPLINE_CURVE((1.02428162962097,1.02311336089458,1.02147610369991))
REPRESENTATION_ITEM('')
);
#851=(
BOUNDED_CURVE()
B_SPLINE_CURVE(2,(#38068,#38069,#38070),.UNSPECIFIED.,.F.,.F.)
B_SPLINE_CURVE_WITH_KNOTS((3,3),(0.218746031477172,0.271795897845358),
 .UNSPECIFIED.)
CURVE()
GEOMETRIC_REPRESENTATION_ITEM()
RATIONAL_B_SPLINE_CURVE((1.02147610369993,1.02311336089461,1.024281629621))
REPRESENTATION_ITEM('')
);
#852=(
BOUNDED_CURVE()
B_SPLINE_CURVE(2,(#38072,#38073,#38074),.UNSPECIFIED.,.F.,.F.)
B_SPLINE_CURVE_WITH_KNOTS((3,3),(0.536094506482398,0.589144372850586),
 .UNSPECIFIED.)
CURVE()
GEOMETRIC_REPRESENTATION_ITEM()
RATIONAL_B_SPLINE_CURVE((1.02428162962101,1.02311336089462,1.02147610369994))
REPRESENTATION_ITEM('')
);
#853=(
BOUNDED_CURVE()
B_SPLINE_CURVE(2,(#38078,#38079,#38080),.UNSPECIFIED.,.F.,.F.)
B_SPLINE_CURVE_WITH_KNOTS((3,3),(0.218746031477161,0.271795897845345),
 .UNSPECIFIED.)
CURVE()
GEOMETRIC_REPRESENTATION_ITEM()
RATIONAL_B_SPLINE_CURVE((1.02147610369992,1.02311336089459,1.02428162962098))
REPRESENTATION_ITEM('')
);
#854=(
BOUNDED_CURVE()
B_SPLINE_CURVE(2,(#38082,#38083,#38084),.UNSPECIFIED.,.F.,.F.)
B_SPLINE_CURVE_WITH_KNOTS((3,3),(0.536094506482393,0.58914437285058),
 .UNSPECIFIED.)
CURVE()
GEOMETRIC_REPRESENTATION_ITEM()
RATIONAL_B_SPLINE_CURVE((1.02428162962098,1.02311336089459,1.02147610369992))
REPRESENTATION_ITEM('')
);
#855=(
BOUNDED_CURVE()
B_SPLINE_CURVE(2,(#38088,#38089,#38090),.UNSPECIFIED.,.F.,.F.)
B_SPLINE_CURVE_WITH_KNOTS((3,3),(0.21874603147716,0.271795897845346),
 .UNSPECIFIED.)
CURVE()
GEOMETRIC_REPRESENTATION_ITEM()
RATIONAL_B_SPLINE_CURVE((1.02147610369996,1.02311336089463,1.02428162962102))
REPRESENTATION_ITEM('')
);
#856=(
BOUNDED_CURVE()
B_SPLINE_CURVE(2,(#38092,#38093,#38094),.UNSPECIFIED.,.F.,.F.)
B_SPLINE_CURVE_WITH_KNOTS((3,3),(0.536094506482404,0.589144372850591),
 .UNSPECIFIED.)
CURVE()
GEOMETRIC_REPRESENTATION_ITEM()
RATIONAL_B_SPLINE_CURVE((1.02428162962101,1.02311336089461,1.02147610369994))
REPRESENTATION_ITEM('')
);
#857=(
BOUNDED_CURVE()
B_SPLINE_CURVE(2,(#38098,#38099,#38100),.UNSPECIFIED.,.F.,.F.)
B_SPLINE_CURVE_WITH_KNOTS((3,3),(0.218746031477173,0.271795897845354),
 .UNSPECIFIED.)
CURVE()
GEOMETRIC_REPRESENTATION_ITEM()
RATIONAL_B_SPLINE_CURVE((1.02147610369983,1.0231133608945,1.02428162962088))
REPRESENTATION_ITEM('')
);
#858=(
BOUNDED_CURVE()
B_SPLINE_CURVE(2,(#38102,#38103,#38104),.UNSPECIFIED.,.F.,.F.)
B_SPLINE_CURVE_WITH_KNOTS((3,3),(0.536094506482412,0.589144372850603),
 .UNSPECIFIED.)
CURVE()
GEOMETRIC_REPRESENTATION_ITEM()
RATIONAL_B_SPLINE_CURVE((1.02428162962111,1.02311336089471,1.02147610370003))
REPRESENTATION_ITEM('')
);
#859=(
BOUNDED_CURVE()
B_SPLINE_CURVE(2,(#38108,#38109,#38110),.UNSPECIFIED.,.F.,.F.)
B_SPLINE_CURVE_WITH_KNOTS((3,3),(0.218746031477171,0.271795897845355),
 .UNSPECIFIED.)
CURVE()
GEOMETRIC_REPRESENTATION_ITEM()
RATIONAL_B_SPLINE_CURVE((1.02147610369989,1.02311336089456,1.02428162962095))
REPRESENTATION_ITEM('')
);
#860=(
BOUNDED_CURVE()
B_SPLINE_CURVE(2,(#38112,#38113,#38114),.UNSPECIFIED.,.F.,.F.)
B_SPLINE_CURVE_WITH_KNOTS((3,3),(0.536094506482401,0.589144372850588),
 .UNSPECIFIED.)
CURVE()
GEOMETRIC_REPRESENTATION_ITEM()
RATIONAL_B_SPLINE_CURVE((1.02428162962099,1.0231133608946,1.02147610369993))
REPRESENTATION_ITEM('')
);
#861=(
BOUNDED_CURVE()
B_SPLINE_CURVE(2,(#38117,#38118,#38119),.UNSPECIFIED.,.F.,.F.)
B_SPLINE_CURVE_WITH_KNOTS((3,3),(0.218746031477171,0.271795897845354),
 .UNSPECIFIED.)
CURVE()
GEOMETRIC_REPRESENTATION_ITEM()
RATIONAL_B_SPLINE_CURVE((1.02147610369987,1.02311336089454,1.02428162962093))
REPRESENTATION_ITEM('')
);
#862=FACE_BOUND('',#2714,.T.);
#863=FACE_BOUND('',#2717,.T.);
#864=FACE_BOUND('',#2779,.T.);
#865=FACE_BOUND('',#2781,.T.);
#866=FACE_BOUND('',#2783,.T.);
#867=FACE_BOUND('',#2785,.T.);
#868=FACE_BOUND('',#2787,.T.);
#869=FACE_BOUND('',#2800,.T.);
#870=FACE_BOUND('',#2805,.T.);
#871=FACE_BOUND('',#2807,.T.);
#872=FACE_BOUND('',#2820,.T.);
#873=FACE_BOUND('',#2823,.T.);
#874=FACE_BOUND('',#2826,.T.);
#875=FACE_BOUND('',#2837,.T.);
#876=FACE_BOUND('',#2871,.T.);
#877=FACE_BOUND('',#2873,.T.);
#878=FACE_BOUND('',#2883,.T.);
#879=FACE_BOUND('',#2902,.T.);
#880=FACE_BOUND('',#2904,.T.);
#881=FACE_BOUND('',#2914,.T.);
#882=FACE_BOUND('',#2916,.T.);
#883=FACE_BOUND('',#2951,.T.);
#884=FACE_BOUND('',#2953,.T.);
#885=FACE_BOUND('',#3017,.T.);
#886=FACE_BOUND('',#3018,.T.);
#887=FACE_BOUND('',#3023,.T.);
#888=FACE_BOUND('',#3024,.T.);
#889=FACE_BOUND('',#3026,.T.);
#890=FACE_BOUND('',#3028,.T.);
#891=FACE_BOUND('',#3032,.T.);
#892=FACE_BOUND('',#3041,.T.);
#893=FACE_BOUND('',#3047,.T.);
#894=FACE_BOUND('',#3098,.T.);
#895=FACE_BOUND('',#3100,.T.);
#896=FACE_BOUND('',#3103,.T.);
#897=FACE_BOUND('',#3107,.T.);
#898=FACE_BOUND('',#3109,.T.);
#899=FACE_BOUND('',#3111,.T.);
#900=FACE_BOUND('',#3114,.T.);
#901=FACE_BOUND('',#3116,.T.);
#902=FACE_BOUND('',#3120,.T.);
#903=FACE_BOUND('',#3248,.T.);
#904=FACE_BOUND('',#3413,.T.);
#905=FACE_BOUND('',#3540,.T.);
#906=FACE_BOUND('',#3542,.T.);
#907=B_SPLINE_CURVE_WITH_KNOTS('',3,(#24912,#24913,#24914,#24915,#24916,
#24917,#24918,#24919,#24920,#24921,#24922,#24923,#24924,#24925,#24926,#24927,
#24928,#24929,#24930,#24931,#24932,#24933,#24934,#24935,#24936,#24937,#24938,
#24939,#24940,#24941,#24942,#24943,#24944,#24945),.UNSPECIFIED.,.T.,.F.,
(4,2,2,2,2,2,2,2,2,2,2,2,2,2,2,2,4),(-1.57949026336004,-1.48075154424537,
-1.38201282513069,-1.28331526132536,-1.18461769752003,-1.08592013371471,
-0.98722256990938,-0.888483850794701,-0.789745131680022,-0.691006412565344,
-0.592267693450665,-0.493570129645338,-0.394872565840011,-0.296175002034684,
-0.197477438229357,-0.0987387191146787,0.),.UNSPECIFIED.);
#908=B_SPLINE_CURVE_WITH_KNOTS('',3,(#25706,#25707,#25708,#25709,#25710,
#25711,#25712,#25713,#25714,#25715,#25716,#25717,#25718,#25719,#25720,#25721,
#25722,#25723,#25724,#25725,#25726,#25727,#25728,#25729,#25730,#25731,#25732,
#25733,#25734,#25735,#25736,#25737,#25738,#25739,#25740,#25741),
 .UNSPECIFIED.,.F.,.F.,(4,2,2,2,2,2,2,2,2,2,2,2,2,2,2,2,2,4),(0.,0.0855939099291143,
0.17410949539989,0.337900796524859,0.497108066486332,0.656524415442333,
0.820403798482143,0.977076652433585,1.1382988894702,1.30211536903791,1.45920718825481,
1.6223913309354,1.78298213056648,1.94186476292235,2.10710718046966,2.26419884117872,
2.42492153336099,2.58541477279612),.UNSPECIFIED.);
#909=B_SPLINE_CURVE_WITH_KNOTS('',3,(#25747,#25748,#25749,#25750,#25751,
#25752,#25753,#25754,#25755,#25756,#25757,#25758,#25759,#25760,#25761,#25762,
#25763,#25764,#25765,#25766,#25767,#25768,#25769,#25770,#25771,#25772,#25773,
#25774,#25775,#25776,#25777,#25778,#25779,#25780,#25781,#25782),
 .UNSPECIFIED.,.F.,.F.,(4,2,2,2,2,2,2,2,2,2,2,2,2,2,2,2,2,4),(60.7773622036861,
60.7984307512578,60.9623015973858,61.1221066343054,61.2805211858834,61.444748688821,
61.6027543469895,61.7661864642053,61.9283577950001,62.0848598014743,62.2487106901294,
62.4090254078727,62.5666049251944,62.7313988978381,62.889895395675,63.0516314776395,
63.2095616444729,63.3630379643741),.UNSPECIFIED.);
#910=B_SPLINE_CURVE_WITH_KNOTS('',3,(#25785,#25786,#25787,#25788,#25789,
#25790,#25791,#25792,#25793,#25794,#25795,#25796,#25797,#25798,#25799,#25800,
#25801,#25802,#25803,#25804,#25805,#25806,#25807,#25808,#25809,#25810,#25811,
#25812,#25813,#25814,#25815,#25816,#25817,#25818,#25819,#25820,#25821,#25822),
 .UNSPECIFIED.,.F.,.F.,(4,2,2,2,2,2,2,2,2,2,2,2,2,2,2,2,2,2,4),(2.58541477279612,
2.58875674058881,2.74542529180111,2.90803801163507,3.07013217269297,3.22851746172615,
3.39318279931958,3.55092904348818,3.71112742512023,3.87498226727406,4.0314645454848,
4.19351122166086,4.35734638384252,4.51524546689183,4.67935054595871,4.83797716078043,
4.99767285707326,5.1615476489584,5.1855645153609),.UNSPECIFIED.);
#911=B_SPLINE_CURVE_WITH_KNOTS('',3,(#25827,#25828,#25829,#25830,#25831,
#25832,#25833,#25834,#25835,#25836,#25837,#25838,#25839,#25840,#25841,#25842,
#25843,#25844,#25845,#25846,#25847,#25848,#25849,#25850,#25851,#25852,#25853,
#25854,#25855,#25856,#25857,#25858,#25859,#25860,#25861,#25862),
 .UNSPECIFIED.,.F.,.F.,(4,2,2,2,2,2,2,2,2,2,2,2,2,2,2,2,2,4),(58.1771396961264,
58.224613592811,58.3897391041826,58.5485203454945,58.7093619904073,58.8724312620513,
59.0294255289243,59.1932370819247,59.3543749967249,59.5111139777451,59.6750046303897,
59.8343399231803,59.9937618262344,60.1574607072996,60.315005213044,60.4802904170643,
60.6419193578722,60.7773622036861),.UNSPECIFIED.);
#912=B_SPLINE_CURVE_WITH_KNOTS('',3,(#25863,#25864,#25865,#25866,#25867,
#25868,#25869,#25870,#25871,#25872,#25873,#25874,#25875,#25876,#25877,#25878,
#25879,#25880,#25881,#25882,#25883,#25884,#25885,#25886,#25887,#25888,#25889,
#25890,#25891,#25892,#25893,#25894,#25895,#25896,#25897,#25898),
 .UNSPECIFIED.,.F.,.F.,(4,2,2,2,2,2,2,2,2,2,2,2,2,2,2,2,2,4),(5.1855645153609,
5.31809241175765,5.47960631614643,5.64345734077483,5.80083607956624,5.96434590256516,
6.12417910937735,6.28334770275447,6.44892428370015,6.60574353245866,6.76677257273097,
6.93059221744087,7.08748561288601,7.25043434000472,7.41159722098884,7.57027369545872,
7.73527696164013,7.78581990814952),.UNSPECIFIED.);
#913=B_SPLINE_CURVE_WITH_KNOTS('',3,(#25903,#25904,#25905,#25906,#25907,
#25908,#25909,#25910,#25911,#25912,#25913,#25914,#25915,#25916,#25917,#25918,
#25919,#25920,#25921,#25922,#25923,#25924,#25925,#25926,#25927,#25928,#25929,
#25930,#25931,#25932,#25933,#25934,#25935,#25936,#25937,#25938),
 .UNSPECIFIED.,.F.,.F.,(4,2,2,2,2,2,2,2,2,2,2,2,2,2,2,2,2,4),(55.5770402575689,
55.6524503192492,55.8164457466301,55.974248469311,56.1384186057709,56.3003534752986,
56.4568207460609,56.620670390864,56.7807635929306,56.9386504233684,57.1031998344716,
57.2614839345338,57.4238795946348,57.5863762730804,57.7429819545077,57.9068118223431,
58.0674272232114,58.1771396961264),.UNSPECIFIED.);
#914=B_SPLINE_CURVE_WITH_KNOTS('',3,(#25939,#25940,#25941,#25942,#25943,
#25944,#25945,#25946,#25947,#25948,#25949,#25950,#25951,#25952,#25953,#25954,
#25955,#25956,#25957,#25958,#25959,#25960,#25961,#25962,#25963,#25964,#25965,
#25966,#25967,#25968,#25969,#25970,#25971,#25972,#25973,#25974),
 .UNSPECIFIED.,.F.,.F.,(4,2,2,2,2,2,2,2,2,2,2,2,2,2,2,2,2,4),(7.78581990814952,
7.89259977417174,8.05310409347892,8.21694253542575,8.37350006053866,8.53587605970679,
8.6986491541994,8.85682980243783,9.0212593655275,9.17933464700114,9.33932036571389,
9.50317869408483,9.65965348486788,9.82147380855276,9.98605555221982,10.1437614501634,
10.307645465901,10.3859883446169),.UNSPECIFIED.);
#915=B_SPLINE_CURVE_WITH_KNOTS('',3,(#25979,#25980,#25981,#25982,#25983,
#25984,#25985,#25986,#25987,#25988,#25989,#25990,#25991,#25992,#25993,#25994,
#25995,#25996,#25997,#25998,#25999,#26000,#26001,#26002,#26003,#26004,#26005,
#26006,#26007,#26008,#26009,#26010,#26011,#26012,#26013,#26014),
 .UNSPECIFIED.,.F.,.F.,(4,2,2,2,2,2,2,2,2,2,2,2,2,2,2,2,2,4),(52.9768680989303,
53.081832297763,53.2446622895934,53.4014648709036,53.5652829780878,53.726203631189,
53.8830974752061,54.0485565057052,54.2076239213249,54.3676916335495,54.5310872191559,
54.6883648994079,54.8521973651977,55.0136084384584,55.1701810570016,55.3340506253698,
55.4936479339503,55.5770402575689),.UNSPECIFIED.);
#916=B_SPLINE_CURVE_WITH_KNOTS('',3,(#26015,#26016,#26017,#26018,#26019,
#26020,#26021,#26022,#26023,#26024,#26025,#26026,#26027,#26028,#26029,#26030,
#26031,#26032,#26033,#26034,#26035,#26036,#26037,#26038,#26039,#26040,#26041,
#26042,#26043,#26044,#26045,#26046,#26047,#26048,#26049,#26050),
 .UNSPECIFIED.,.F.,.F.,(4,2,2,2,2,2,2,2,2,2,2,2,2,2,2,2,2,4),(10.3859883446169,
10.4666739699023,10.6261726770555,10.790050887668,10.946678863482,11.1079867851551,
11.2718131320933,11.4289892727587,11.5922689727822,11.7526295968928,11.9115959323349,
12.0769359936918,12.2339397311091,12.3947517233337,12.5585825995751,12.7153077276059,
12.8780179916939,12.9862583448684),.UNSPECIFIED.);
#917=B_SPLINE_CURVE_WITH_KNOTS('',3,(#26055,#26056,#26057,#26058,#26059,
#26060,#26061,#26062,#26063,#26064,#26065,#26066,#26067,#26068,#26069,#26070,
#26071,#26072,#26073,#26074,#26075,#26076,#26077,#26078,#26079,#26080,#26081,
#26082,#26083,#26084,#26085,#26086,#26087,#26088,#26089,#26090),
 .UNSPECIFIED.,.F.,.F.,(4,2,2,2,2,2,2,2,2,2,2,2,2,2,2,2,2,4),(50.3767904783692,
50.5107812061852,50.6724906071711,50.828973545376,50.9928307396947,51.1527115480716,
51.3109574918724,51.4752705457191,51.6333495951751,51.7964642972003,51.9587226784194,
52.115238606926,52.2790758624476,52.4394709077892,52.5969192615452,52.7618026110902,
52.9203752231922,52.9768680989303),.UNSPECIFIED.);
#918=B_SPLINE_CURVE_WITH_KNOTS('',3,(#26091,#26092,#26093,#26094,#26095,
#26096,#26097,#26098,#26099,#26100,#26101,#26102,#26103,#26104,#26105,#26106,
#26107,#26108,#26109,#26110,#26111,#26112,#26113,#26114,#26115,#26116,#26117,
#26118,#26119,#26120,#26121,#26122,#26123,#26124,#26125,#26126),
 .UNSPECIFIED.,.F.,.F.,(4,2,2,2,2,2,2,2,2,2,2,2,2,2,2,2,2,4),(12.9862583448684,
13.0398334471711,13.198303057029,13.3630660757444,13.5206812995336,13.680967893734,
13.8448182265697,14.0013132076352,14.1634544438297,14.3269766650684,14.4849563935275,
14.6491542481686,14.8076151751952,14.9673935886308,15.1312638796505,15.287780569243,
15.4493815170271,15.5864597642529),.UNSPECIFIED.);
#919=B_SPLINE_CURVE_WITH_KNOTS('',3,(#26131,#26132,#26133,#26134,#26135,
#26136,#26137,#26138,#26139,#26140,#26141,#26142,#26143,#26144,#26145,#26146,
#26147,#26148,#26149,#26150,#26151,#26152,#26153,#26154,#26155,#26156,#26157,
#26158,#26159,#26160,#26161,#26162,#26163,#26164,#26165,#26166),
 .UNSPECIFIED.,.F.,.F.,(4,2,2,2,2,2,2,2,2,2,2,2,2,2,2,2,2,4),(47.7766546378743,
47.9374651673666,48.0981733406384,48.2552750339325,48.4205017209669,48.5793705970124,
48.7399906609457,48.9031593617984,49.060237346639,49.2240500153142,49.3852581718922,
49.5419351947185,49.7058122286832,49.865214957112,50.0244445853918,50.1882207786755,
50.3458320184278,50.3767904783692),.UNSPECIFIED.);
#920=B_SPLINE_CURVE_WITH_KNOTS('',3,(#26167,#26168,#26169,#26170,#26171,
#26172,#26173,#26174,#26175,#26176,#26177,#26178,#26179,#26180,#26181,#26182,
#26183,#26184,#26185,#26186,#26187,#26188,#26189,#26190,#26191,#26192,#26193,
#26194,#26195,#26196,#26197,#26198,#26199,#26200,#26201,#26202,#26203,#26204),
 .UNSPECIFIED.,.F.,.F.,(4,2,2,2,2,2,2,2,2,2,2,2,2,2,2,2,2,2,4),(15.5864597642529,
15.6132408118112,15.7707051340016,15.9343126587632,16.0939249158545,16.2531794243581,
16.4170714994651,16.5738675985109,16.7349219742824,16.8987375458885,17.0556532440191,
17.2186301669557,17.3797093851925,17.5384101242186,17.7034419351815,17.8607275155819,
18.0212576121742,18.1850918696393,18.1866042820843),.UNSPECIFIED.);
#921=B_SPLINE_CURVE_WITH_KNOTS('',3,(#26209,#26210,#26211,#26212,#26213,
#26214,#26215,#26216,#26217,#26218,#26219,#26220,#26221,#26222,#26223,#26224,
#26225,#26226,#26227,#26228,#26229,#26230,#26231,#26232,#26233,#26234,#26235,
#26236,#26237,#26238,#26239,#26240,#26241,#26242,#26243,#26244,#26245,#26246),
 .UNSPECIFIED.,.F.,.F.,(4,2,2,2,2,2,2,2,2,2,2,2,2,2,2,2,2,2,4),(45.1765418699449,
45.2008622875136,45.3647351735005,45.524417367748,45.6830642524393,45.8471544022965,
46.0050402672,46.1689154269324,46.3309469416839,46.4874256817532,46.6512786206368,
46.8114626984097,46.9692247153789,47.1338743924919,47.2922459061876,47.4543757188514,
47.6169728017918,47.7736318836056,47.7766546378743),.UNSPECIFIED.);
#922=B_SPLINE_CURVE_WITH_KNOTS('',3,(#26247,#26248,#26249,#26250,#26251,
#26252,#26253,#26254,#26255,#26256,#26257,#26258,#26259,#26260,#26261,#26262,
#26263,#26264,#26265,#26266,#26267,#26268,#26269,#26270,#26271,#26272,#26273,
#26274,#26275,#26276,#26277,#26278,#26279,#26280,#26281,#26282),
 .UNSPECIFIED.,.F.,.F.,(4,2,2,2,2,2,2,2,2,2,2,2,2,2,2,2,2,4),(18.1866042820843,
18.3416583432495,18.5040624481538,18.6667381565374,18.8249426329171,18.9894000170298,
19.1474252494328,19.3074357342038,19.4712898558371,19.6277597294378,19.7896065096557,
19.9540828346108,20.1118108083518,20.2757204293955,20.4346898301103,20.5942109922705,
20.7580850070076,20.7866467102843),.UNSPECIFIED.);
#923=B_SPLINE_CURVE_WITH_KNOTS('',3,(#26287,#26288,#26289,#26290,#26291,
#26292,#26293,#26294,#26295,#26296,#26297,#26298,#26299,#26300,#26301,#26302,
#26303,#26304,#26305,#26306,#26307,#26308,#26309,#26310,#26311,#26312,#26313,
#26314,#26315,#26316,#26317,#26318,#26319,#26320,#26321,#26322),
 .UNSPECIFIED.,.F.,.F.,(4,2,2,2,2,2,2,2,2,2,2,2,2,2,2,2,2,4),(42.5763202365159,
42.6272137044713,42.7922006287403,42.9508628372109,43.1120609046234,43.2749934789742,
43.4318737653827,43.5956919693039,43.7567061916774,43.9135330874799,44.0790936811999,
44.2382483942517,44.3981092173091,44.5616035062386,44.7189684127531,44.8828158463609,
45.0443156631371,45.1765418699449),.UNSPECIFIED.);
#924=B_SPLINE_CURVE_WITH_KNOTS('',3,(#26323,#26324,#26325,#26326,#26327,
#26328,#26329,#26330,#26331,#26332,#26333,#26334,#26335,#26336,#26337,#26338,
#26339,#26340,#26341,#26342,#26343,#26344,#26345,#26346,#26347,#26348,#26349,
#26350,#26351,#26352,#26353,#26354,#26355,#26356,#26357,#26358),
 .UNSPECIFIED.,.F.,.F.,(4,2,2,2,2,2,2,2,2,2,2,2,2,2,2,2,2,4),(20.7866467102843,
20.9146963524292,21.0760277965509,21.2398535490734,21.3970528690657,21.5603592074625,
21.7206442282256,21.879633563418,22.0450009494638,22.2019744509748,22.3628112483055,
22.5266369147414,22.6833780419026,22.8461157700061,23.0078396944665,23.1663326694566,
23.3311232209272,23.3868406765007),.UNSPECIFIED.);
#925=B_SPLINE_CURVE_WITH_KNOTS('',3,(#26363,#26364,#26365,#26366,#26367,
#26368,#26369,#26370,#26371,#26372,#26373,#26374,#26375,#26376,#26377,#26378,
#26379,#26380,#26381,#26382,#26383,#26384,#26385,#26386,#26387,#26388,#26389,
#26390,#26391,#26392,#26393,#26394,#26395,#26396,#26397,#26398),
 .UNSPECIFIED.,.F.,.F.,(4,2,2,2,2,2,2,2,2,2,2,2,2,2,2,2,2,4),(39.976181354914,
40.0548545094264,40.2187235993922,40.3764162958879,40.5410428736157,40.7028479160014,
40.8593220347091,41.0231789792917,41.183150212704,41.3412453402344,41.5056589319328,
41.6638255482828,41.8266399717696,41.9889998998425,42.1455504461389,42.3093874956531,
42.469876832279,42.5763202365159),.UNSPECIFIED.);
#926=B_SPLINE_CURVE_WITH_KNOTS('',3,(#26399,#26400,#26401,#26402,#26403,
#26404,#26405,#26406,#26407,#26408,#26409,#26410,#26411,#26412,#26413,#26414,
#26415,#26416,#26417,#26418,#26419,#26420,#26421,#26422,#26423,#26424,#26425,
#26426,#26427,#26428,#26429,#26430,#26431,#26432,#26433,#26434),
 .UNSPECIFIED.,.F.,.F.,(4,2,2,2,2,2,2,2,2,2,2,2,2,2,2,2,2,4),(23.3868406765007,
23.4886942399868,23.6490054702219,23.8128505253174,23.9693475111746,24.131515447711,
24.294934472013,24.4529365506312,24.6171605508436,24.7755657085432,24.9353671583331,
25.0992321700508,25.2557375472926,25.4173629469987,25.5826345980646,25.7401753747385,
25.9038705675823,25.9870085755541),.UNSPECIFIED.);
#927=B_SPLINE_CURVE_WITH_KNOTS('',3,(#26439,#26440,#26441,#26442,#26443,
#26444,#26445,#26446,#26447,#26448,#26449,#26450,#26451,#26452,#26453,#26454,
#26455,#26456,#26457,#26458,#26459,#26460,#26461,#26462,#26463,#26464,#26465,
#26466,#26467,#26468,#26469,#26470,#26471,#26472,#26473,#26474),
 .UNSPECIFIED.,.F.,.F.,(4,2,2,2,2,2,2,2,2,2,2,2,2,2,2,2,2,4),(37.3759376529246,
37.4845427362404,37.6472373015768,37.8039522835337,37.9677822299911,38.1285797555106,
38.2855942839381,38.4509186393567,38.6098713537324,38.7702632861893,38.9335276219079,
39.0906900865903,39.2545134241937,39.4158074320668,39.572440014719,39.7363168360909,
39.8958021421056,39.976181354914),.UNSPECIFIED.);
#928=B_SPLINE_CURVE_WITH_KNOTS('',3,(#26475,#26476,#26477,#26478,#26479,
#26480,#26481,#26482,#26483,#26484,#26485,#26486,#26487,#26488,#26489,#26490,
#26491,#26492,#26493,#26494,#26495,#26496,#26497,#26498,#26499,#26500,#26501,
#26502,#26503,#26504,#26505,#26506,#26507,#26508,#26509,#26510),
 .UNSPECIFIED.,.F.,.F.,(4,2,2,2,2,2,2,2,2,2,2,2,2,2,2,2,2,4),(25.9870085755541,
26.0632825128444,26.2226140300249,26.3864988483248,26.5432310331721,26.7043651749984,
26.8681708361658,27.0251614375154,27.1882270747621,27.3490576030318,27.5078350894429,
27.6729569285989,27.8301355116954,27.9907472073234,28.1545711733677,28.311172302475,
28.4736653813112,28.5871150949191),.UNSPECIFIED.);
#929=B_SPLINE_CURVE_WITH_KNOTS('',3,(#26515,#26516,#26517,#26518,#26519,
#26520,#26521,#26522,#26523,#26524,#26525,#26526,#26527,#26528,#26529,#26530,
#26531,#26532,#26533,#26534,#26535,#26536,#26537,#26538,#26539,#26540,#26541,
#26542,#26543,#26544,#26545,#26546,#26547,#26548,#26549,#26550),
 .UNSPECIFIED.,.F.,.F.,(4,2,2,2,2,2,2,2,2,2,2,2,2,2,2,2,2,4),(34.7757588841055,
34.9131766642864,35.0747633517156,35.2312822366005,35.3951516261494,35.5549164450714,
35.7133996037316,35.8775823658074,36.0355488361476,36.1991146383398,36.3612405616305,
36.5177317480541,36.68158117977,36.8418534210273,36.9994857262212,37.1642329854863,
37.3226888436329,37.3759376529246),.UNSPECIFIED.);
#930=B_SPLINE_CURVE_WITH_KNOTS('',3,(#26551,#26552,#26553,#26554,#26555,
#26556,#26557,#26558,#26559,#26560,#26561,#26562,#26563,#26564,#26565,#26566,
#26567,#26568,#26569,#26570,#26571,#26572,#26573,#26574,#26575,#26576,#26577,
#26578,#26579,#26580,#26581,#26582,#26583,#26584,#26585,#26586),
 .UNSPECIFIED.,.F.,.F.,(4,2,2,2,2,2,2,2,2,2,2,2,2,2,2,2,2,4),(28.5871150949191,
28.6360488595124,28.7943292099721,28.9588749397764,29.1167530356116,29.2768424992895,
29.4406862391693,29.5971479886017,29.7590791830785,29.9232364301957,30.0810353144069,
30.2450269438081,30.4038198713806,30.5634133135096,30.7272769768795,30.883843214224,
31.0452504411699,31.1870971694932),.UNSPECIFIED.);
#931=B_SPLINE_CURVE_WITH_KNOTS('',3,(#26591,#26592,#26593,#26594,#26595,
#26596,#26597,#26598,#26599,#26600,#26601,#26602,#26603,#26604,#26605,#26606,
#26607,#26608,#26609,#26610,#26611,#26612,#26613,#26614,#26615,#26616,#26617,
#26618,#26619,#26620,#26621,#26622,#26623,#26624,#26625,#26626,#26627,#26628),
 .UNSPECIFIED.,.F.,.F.,(4,2,2,2,2,2,2,2,2,2,2,2,2,2,2,2,2,2,4),(32.175633435784,
32.1775107813409,32.3413446580404,32.501860016056,32.6591611046315,32.8241767832933,
32.9828635414385,33.1439805221191,33.3069415147973,33.4638441163799,33.6276592531707,
33.7886991048983,33.9455039498272,34.1093951733975,34.2686355916604,34.4282781528139,
34.5918698348922,34.7493201518321,34.7757588841055),.UNSPECIFIED.);
#932=B_SPLINE_CURVE_WITH_KNOTS('',3,(#26629,#26630,#26631,#26632,#26633,
#26634,#26635,#26636,#26637,#26638,#26639,#26640,#26641,#26642,#26643,#26644,
#26645,#26646,#26647,#26648,#26649,#26650,#26651,#26652,#26653,#26654,#26655,
#26656,#26657,#26658,#26659,#26660,#26661,#26662,#26663,#26664,#26665,#26666),
 .UNSPECIFIED.,.F.,.F.,(4,2,2,2,2,2,2,2,2,2,2,2,2,2,2,2,2,2,4),(31.1870971694932,
31.2090772686752,31.3663512188482,31.5297431143764,31.6898001409927,31.8488637597776,
32.0143190871344,32.1712055862005,32.3321225158812,32.4959346463123,32.6527332075193,
32.814331120641,32.970833571967,33.1346911409304,33.294466191355,33.4528984815721,
33.6170936754505,33.7750699448881,33.787031069066),.UNSPECIFIED.);
#933=B_SPLINE_CURVE_WITH_KNOTS('',3,(#26671,#26672,#26673,#26674,#26675,
#26676,#26677,#26678,#26679,#26680,#26681,#26682,#26683,#26684,#26685,#26686,
#26687,#26688,#26689,#26690,#26691,#26692,#26693,#26694,#26695,#26696,#26697,
#26698,#26699,#26700,#26701,#26702,#26703,#26704,#26705,#26706),
 .UNSPECIFIED.,.F.,.F.,(4,2,2,2,2,2,2,2,2,2,2,2,2,2,2,2,2,4),(29.5756035802014,
29.6045003448811,29.7683739842147,29.9278820022522,30.0868774516155,30.2507723498575,
30.4084873914971,30.5730119648943,30.7348436465841,30.8913135094951,31.0551672611946,
31.2151634914049,31.3732104004737,31.537651997735,31.6958427008405,31.8585627767629,
32.0209509921586,32.175633435784),.UNSPECIFIED.);
#934=B_SPLINE_CURVE_WITH_KNOTS('',3,(#26707,#26708,#26709,#26710,#26711,
#26712,#26713,#26714,#26715,#26716,#26717,#26718,#26719,#26720,#26721,#26722,
#26723,#26724,#26725,#26726,#26727,#26728,#26729,#26730,#26731,#26732,#26733,
#26734,#26735,#26736,#26737,#26738,#26739,#26740,#26741,#26742),
 .UNSPECIFIED.,.F.,.F.,(4,2,2,2,2,2,2,2,2,2,2,2,2,2,2,2,2,4),(33.787031069066,
33.9385479563215,34.1006868518737,34.2571718625092,34.42100947491,34.5812931938916,
34.7388835311519,34.9036443059465,35.0621107580024,35.2238858328536,35.3865939729145,
35.5433136155739,35.7071317939495,35.8679409387723,36.0249243123382,36.1902620337357,
36.3492250687649,36.3870506062284),.UNSPECIFIED.);
#935=B_SPLINE_CURVE_WITH_KNOTS('',3,(#26747,#26748,#26749,#26750,#26751,
#26752,#26753,#26754,#26755,#26756,#26757,#26758,#26759,#26760,#26761,#26762,
#26763,#26764,#26765,#26766,#26767,#26768,#26769,#26770,#26771,#26772,#26773,
#26774,#26775,#26776,#26777,#26778,#26779,#26780,#26781,#26782),
 .UNSPECIFIED.,.F.,.F.,(4,2,2,2,2,2,2,2,2,2,2,2,2,2,2,2,2,4),(26.9754188903882,
27.0315113171753,27.1962861825211,27.3547655743049,27.5165311558328,27.6792532653912,
27.8359842958766,27.9998100765242,28.1606325684036,28.3176182504787,28.4829700532874,
28.6419459835266,28.8022649856762,28.9655561057364,29.1227419640259,29.2865656025431,
29.4478833589509,29.5756035802014),.UNSPECIFIED.);
#936=B_SPLINE_CURVE_WITH_KNOTS('',3,(#26783,#26784,#26785,#26786,#26787,
#26788,#26789,#26790,#26791,#26792,#26793,#26794,#26795,#26796,#26797,#26798,
#26799,#26800,#26801,#26802,#26803,#26804,#26805,#26806,#26807,#26808,#26809,
#26810,#26811,#26812,#26813,#26814,#26815,#26816,#26817,#26818),
 .UNSPECIFIED.,.F.,.F.,(4,2,2,2,2,2,2,2,2,2,2,2,2,2,2,2,2,4),(36.3870506062284,
36.5095505106562,36.6728277922848,36.8300008138566,36.9938159430349,37.1551205776933,
37.3117325973914,37.4755984325684,37.6350936337405,37.7940923476327,37.957973577995,
38.1156759713782,38.2802126316001,38.4420305861104,38.5984931880261,38.7623391387606,
38.9223220705895,38.9870541035935),.UNSPECIFIED.);
#937=B_SPLINE_CURVE_WITH_KNOTS('',3,(#26823,#26824,#26825,#26826,#26827,
#26828,#26829,#26830,#26831,#26832,#26833,#26834,#26835,#26836,#26837,#26838,
#26839,#26840,#26841,#26842,#26843,#26844,#26845,#26846,#26847,#26848,#26849,
#26850,#26851,#26852,#26853,#26854,#26855,#26856,#26857,#26858),
 .UNSPECIFIED.,.F.,.F.,(4,2,2,2,2,2,2,2,2,2,2,2,2,2,2,2,2,4),(24.3752567166036,
24.4565959364233,24.6172359201442,24.781068110726,24.9376878811401,25.1002110361017,
25.2625412882476,25.4208485741219,25.5854244165739,25.743280986078,25.9033982265957,
26.0672501674617,26.2237210788033,26.3856814121459,26.5497791793857,26.7136243818014,
26.8739213856385,26.9754188903882),.UNSPECIFIED.);
#938=B_SPLINE_CURVE_WITH_KNOTS('',3,(#26859,#26860,#26861,#26862,#26863,
#26864,#26865,#26866,#26867,#26868,#26869,#26870,#26871,#26872,#26873,#26874,
#26875,#26876,#26877,#26878,#26879,#26880,#26881,#26882,#26883,#26884,#26885,
#26886,#26887,#26888,#26889,#26890,#26891,#26892,#26893,#26894),
 .UNSPECIFIED.,.F.,.F.,(4,2,2,2,2,2,2,2,2,2,2,2,2,2,2,2,2,4),(38.9870541035935,
39.0803705159472,39.2447979793195,39.4029756632131,39.5657063457729,39.7280804788507,
39.8846302741835,40.0484563466386,40.2089581787015,40.3662583228638,40.5312596936028,
40.6899333193432,40.8510582940319,41.014005155137,41.1708951149417,41.3347024266529,
41.495728810533,41.5870777147423),.UNSPECIFIED.);
#939=B_SPLINE_CURVE_WITH_KNOTS('',3,(#26899,#26900,#26901,#26902,#26903,
#26904,#26905,#26906,#26907,#26908,#26909,#26910,#26911,#26912,#26913,#26914,
#26915,#26916,#26917,#26918,#26919,#26920,#26921,#26922,#26923,#26924,#26925,
#26926,#26927,#26928,#26929,#26930,#26931,#26932,#26933,#26934),
 .UNSPECIFIED.,.F.,.F.,(4,2,2,2,2,2,2,2,2,2,2,2,2,2,2,2,2,4),(21.7751553262989,
21.8822756137629,22.0439113791663,22.2090980146475,22.3666462235154,22.5303509413377,
22.6897109077896,22.8490499085509,23.012923595653,23.1696335579083,23.3307757123397,
23.4945773891925,23.6515904448586,23.8146860274203,23.9754731163525,24.1342776665709,
24.2994299151046,24.3752567166036),.UNSPECIFIED.);
#940=B_SPLINE_CURVE_WITH_KNOTS('',3,(#26935,#26936,#26937,#26938,#26939,
#26940,#26941,#26942,#26943,#26944,#26945,#26946,#26947,#26948,#26949,#26950,
#26951,#26952,#26953,#26954,#26955,#26956,#26957,#26958,#26959,#26960,#26961,
#26962,#26963,#26964,#26965,#26966,#26967,#26968,#26969,#26970),
 .UNSPECIFIED.,.F.,.F.,(4,2,2,2,2,2,2,2,2,2,2,2,2,2,2,2,2,4),(41.5870777147423,
41.6525299655238,41.8164131898957,41.9756404002719,42.1352879802968,42.298865531762,
42.4563027572898,42.6201504819589,42.7817237805508,42.9382363008472,43.1020976718053,
43.2618494583129,43.4203343808643,43.5845032887473,43.7424569469071,43.9060330407087,
44.0681451134247,44.1871553710452),.UNSPECIFIED.);
#941=B_SPLINE_CURVE_WITH_KNOTS('',3,(#26975,#26976,#26977,#26978,#26979,
#26980,#26981,#26982,#26983,#26984,#26985,#26986,#26987,#26988,#26989,#26990,
#26991,#26992,#26993,#26994,#26995,#26996,#26997,#26998,#26999,#27000,#27001,
#27002,#27003,#27004,#27005,#27006,#27007,#27008,#27009,#27010),
 .UNSPECIFIED.,.F.,.F.,(4,2,2,2,2,2,2,2,2,2,2,2,2,2,2,2,2,4),(19.1751960155601,
19.3101100041855,19.4728601071602,19.6345116693977,19.7930142851345,19.957817190375,
20.1153499099463,20.2756716296436,20.4395055506287,20.595997428871,20.7581772725523,
20.9215153105913,21.0795263704231,21.2437618078274,21.4021202185422,21.5619310799127,
21.725784954197,21.7751553262989),.UNSPECIFIED.);
#942=B_SPLINE_CURVE_WITH_KNOTS('',3,(#27011,#27012,#27013,#27014,#27015,
#27016,#27017,#27018,#27019,#27020,#27021,#27022,#27023,#27024,#27025,#27026,
#27027,#27028,#27029,#27030,#27031,#27032,#27033,#27034,#27035,#27036,#27037,
#27038,#27039,#27040,#27041,#27042,#27043,#27044,#27045,#27046),
 .UNSPECIFIED.,.F.,.F.,(4,2,2,2,2,2,2,2,2,2,2,2,2,2,2,2,2,4),(44.1871553710452,
44.2246274834992,44.3884688978133,44.5487277671559,44.7063597731386,44.8710928730091,
45.0295356890391,45.1913978592965,45.3540783838714,45.5107819285521,45.6746038470453,
45.835387924594,45.9923996031062,46.1577097889147,46.3166494871573,46.4770468473187,
46.6402972479939,46.7872229415117),.UNSPECIFIED.);
#943=B_SPLINE_CURVE_WITH_KNOTS('',3,(#27051,#27052,#27053,#27054,#27055,
#27056,#27057,#27058,#27059,#27060,#27061,#27062,#27063,#27064,#27065,#27066,
#27067,#27068,#27069,#27070,#27071,#27072,#27073,#27074,#27075,#27076,#27077,
#27078,#27079,#27080,#27081,#27082,#27083,#27084,#27085,#27086,#27087,#27088),
 .UNSPECIFIED.,.F.,.F.,(4,2,2,2,2,2,2,2,2,2,2,2,2,2,2,2,2,2,4),(16.5752364738999,
16.5809043992186,16.738641033749,16.9025615621065,17.0614820445148,17.2210120734106,
17.384875732046,17.5414685495772,17.7028095566869,17.8666275515996,18.0238363732713,
18.1871544175959,18.3473786463044,18.5063772919755,18.6717568025283,18.8287020750767,
18.989549409536,19.1533639946529,19.1751960155601),.UNSPECIFIED.);
#944=B_SPLINE_CURVE_WITH_KNOTS('',3,(#27089,#27090,#27091,#27092,#27093,
#27094,#27095,#27096,#27097,#27098,#27099,#27100,#27101,#27102,#27103,#27104,
#27105,#27106,#27107,#27108,#27109,#27110,#27111,#27112,#27113,#27114,#27115,
#27116,#27117,#27118,#27119,#27120,#27121,#27122,#27123,#27124,#27125,#27126),
 .UNSPECIFIED.,.F.,.F.,(4,2,2,2,2,2,2,2,2,2,2,2,2,2,2,2,2,2,4),(46.7872229415117,
46.7974467558072,46.9612612134908,47.1225419740756,47.279169178961,47.4430377815618,
47.6025101340063,47.7615649335297,47.9254202372429,48.083100144397,48.2477375280673,
48.4095287324009,48.5659953165688,48.7298440455678,48.8898018523219,49.0478978172873,
49.2122971621086,49.370450620887,49.3871486091453),.UNSPECIFIED.);
#945=B_SPLINE_CURVE_WITH_KNOTS('',3,(#27131,#27132,#27133,#27134,#27135,
#27136,#27137,#27138,#27139,#27140,#27141,#27142,#27143,#27144,#27145,#27146,
#27147,#27148,#27149,#27150,#27151,#27152,#27153,#27154,#27155,#27156,#27157,
#27158,#27159,#27160,#27161,#27162,#27163,#27164,#27165,#27166),
 .UNSPECIFIED.,.F.,.F.,(4,2,2,2,2,2,2,2,2,2,2,2,2,2,2,2,2,4),(13.9753192948077,
14.0067045743461,14.1654153988763,14.3304600567658,14.4877125732657,14.6482537657069,
14.8120776792938,14.9686439321478,15.1310607227353,15.2936603060804,15.4518746263024,
15.6163444221346,15.7743273673789,15.9343483004934,16.098192059448,16.2546518382711,
16.4165102067085,16.5752364738999),.UNSPECIFIED.);
#946=B_SPLINE_CURVE_WITH_KNOTS('',3,(#27167,#27168,#27169,#27170,#27171,
#27172,#27173,#27174,#27175,#27176,#27177,#27178,#27179,#27180,#27181,#27182,
#27183,#27184,#27185,#27186,#27187,#27188,#27189,#27190,#27191,#27192,#27193,
#27194,#27195,#27196,#27197,#27198,#27199,#27200,#27201,#27202),
 .UNSPECIFIED.,.F.,.F.,(4,2,2,2,2,2,2,2,2,2,2,2,2,2,2,2,2,4),(49.3871486091453,
49.5332745128823,49.6956202467741,49.8521606598271,50.0159894913195,50.1764651674857,
50.3338005374518,50.4987730301628,50.6574219569031,50.8186270526262,50.9815453671276,
51.138412973096,51.3022229403195,51.4632235408708,51.6200463160427,51.7855925924826,
51.9447341554513,51.9871887418935),.UNSPECIFIED.);
#947=B_SPLINE_CURVE_WITH_KNOTS('',3,(#27207,#27208,#27209,#27210,#27211,
#27212,#27213,#27214,#27215,#27216,#27217,#27218,#27219,#27220,#27221,#27222,
#27223,#27224,#27225,#27226,#27227,#27228,#27229,#27230,#27231,#27232,#27233,
#27234,#27235,#27236,#27237,#27238,#27239,#27240,#27241,#27242),
 .UNSPECIFIED.,.F.,.F.,(4,2,2,2,2,2,2,2,2,2,2,2,2,2,2,2,2,4),(11.3752281506608,
11.4331440082726,11.5928714158197,11.7567340594759,11.9132545003004,12.074802135132,
12.2403347218686,12.3978092052149,12.561429194959,12.7209864699398,12.8802511578905,
13.0441335836658,13.2009066387116,13.3619717253299,13.525777036828,13.6827019191146,
13.8456915128137,13.9753192948077),.UNSPECIFIED.);
#948=B_SPLINE_CURVE_WITH_KNOTS('',3,(#27243,#27244,#27245,#27246,#27247,
#27248,#27249,#27250,#27251,#27252,#27253,#27254,#27255,#27256,#27257,#27258,
#27259,#27260,#27261,#27262,#27263,#27264,#27265,#27266,#27267,#27268,#27269,
#27270,#27271,#27272,#27273,#27274,#27275,#27276,#27277,#27278),
 .UNSPECIFIED.,.F.,.F.,(4,2,2,2,2,2,2,2,2,2,2,2,2,2,2,2,2,4),(51.9871887418935,
52.1045989553424,52.2680792084208,52.4254310665492,52.5892693766665,52.7507558469993,
52.9072959719357,53.0711604271069,53.2308295999598,53.3894774879068,53.5535538206852,
53.7114268637422,53.8753109335028,54.037328629624,54.193798648683,54.3576431588387,
54.5178138567586,54.5872639586609),.UNSPECIFIED.);
#949=B_SPLINE_CURVE_WITH_KNOTS('',3,(#27283,#27284,#27285,#27286,#27287,
#27288,#27289,#27290,#27291,#27292,#27293,#27294,#27295,#27296,#27297,#27298,
#27299,#27300,#27301,#27302,#27303,#27304,#27305,#27306,#27307,#27308,#27309,
#27310,#27311,#27312,#27313,#27314,#27315,#27316,#27317,#27318),
 .UNSPECIFIED.,.F.,.F.,(4,2,2,2,2,2,2,2,2,2,2,2,2,2,2,2,2,4),(8.77513878253031,
8.85957795966849,9.02033579080828,9.1841589294471,9.34084550443931,9.50349734972825,
9.66544094625724,9.82385895709363,9.98856332188794,10.1462334324883,10.3064663402911,
10.4703090291096,10.626787297808,10.7888715304564,10.9525392357421,11.1104691365834,
11.2746107142529,11.3752281506608),.UNSPECIFIED.);
#950=B_SPLINE_CURVE_WITH_KNOTS('',3,(#27319,#27320,#27321,#27322,#27323,
#27324,#27325,#27326,#27327,#27328,#27329,#27330,#27331,#27332,#27333,#27334,
#27335,#27336,#27337,#27338,#27339,#27340,#27341,#27342,#27343,#27344,#27345,
#27346,#27347,#27348,#27349,#27350,#27351,#27352,#27353,#27354),
 .UNSPECIFIED.,.F.,.F.,(4,2,2,2,2,2,2,2,2,2,2,2,2,2,2,2,2,4),(54.5872639586609,
54.6755750711845,54.8402105986611,54.9985690338287,55.1607060588628,55.3232890958237,
55.4799369962627,55.6437618441001,55.8044565200012,55.9615550736393,56.1267675505751,
56.285623328814,56.4462480452348,56.6094027495969,56.7664676863386,56.9302711419498,
57.0914659561543,57.1873615863288),.UNSPECIFIED.);
#951=B_SPLINE_CURVE_WITH_KNOTS('',3,(#27359,#27360,#27361,#27362,#27363,
#27364,#27365,#27366,#27367,#27368,#27369,#27370,#27371,#27372,#27373,#27374,
#27375,#27376,#27377,#27378,#27379,#27380,#27381,#27382,#27383,#27384,#27385,
#27386,#27387,#27388,#27389,#27390,#27391,#27392,#27393,#27394),
 .UNSPECIFIED.,.F.,.F.,(4,2,2,2,2,2,2,2,2,2,2,2,2,2,2,2,2,4),(6.17506899243254,
6.28542206375772,6.44718527831052,6.61191749423575,6.76957357592004,6.93340167664995,
7.09250849583087,7.25195667231655,7.41582556755354,7.57246560060843,7.7337211992204,
7.897532695118,8.05465744283474,8.21787978367144,8.37834425273139,8.537259359205,
8.70254085846295,8.77513878253031),.UNSPECIFIED.);
#952=B_SPLINE_CURVE_WITH_KNOTS('',3,(#27395,#27396,#27397,#27398,#27399,
#27400,#27401,#27402,#27403,#27404,#27405,#27406,#27407,#27408,#27409,#27410,
#27411,#27412,#27413,#27414,#27415,#27416,#27417,#27418,#27419,#27420,#27421,
#27422,#27423,#27424,#27425,#27426,#27427,#27428,#27429,#27430),
 .UNSPECIFIED.,.F.,.F.,(4,2,2,2,2,2,2,2,2,2,2,2,2,2,2,2,2,4),(57.1873615863288,
57.2481374311781,57.412005851322,57.5713955105336,57.7306270023818,57.8943893060583,
58.051987626823,58.2169466622617,58.3786421174995,58.5351175364027,58.6989661200439,
58.8588333669063,59.0170797936999,59.1813784709152,59.3394442077022,59.50256768913,
59.6648117339904,59.7873029751542),.UNSPECIFIED.);
#953=B_SPLINE_CURVE_WITH_KNOTS('',3,(#27435,#27436,#27437,#27438,#27439,
#27440,#27441,#27442,#27443,#27444,#27445,#27446,#27447,#27448,#27449,#27450,
#27451,#27452,#27453,#27454,#27455,#27456,#27457,#27458,#27459,#27460,#27461,
#27462,#27463,#27464,#27465,#27466,#27467,#27468,#27469,#27470),
 .UNSPECIFIED.,.F.,.F.,(4,2,2,2,2,2,2,2,2,2,2,2,2,2,2,2,2,4),(3.57510705038708,
3.71339809964079,3.87628653037861,4.03756721491112,4.19619004676284,4.36113233712773,
4.5185000268825,4.67894820506975,4.84277732466363,4.99930711704217,5.16162319475703,
5.32453503301027,5.48266292720209,5.64703288620151,5.8051728690298,5.9651042464861,
6.1289532790101,6.17506899243254),.UNSPECIFIED.);
#954=B_SPLINE_CURVE_WITH_KNOTS('',3,(#27471,#27472,#27473,#27474,#27475,
#27476,#27477,#27478,#27479,#27480,#27481,#27482,#27483,#27484,#27485,#27486,
#27487,#27488,#27489,#27490,#27491,#27492,#27493,#27494,#27495,#27496,#27497,
#27498,#27499,#27500,#27501,#27502,#27503,#27504,#27505,#27506),
 .UNSPECIFIED.,.F.,.F.,(4,2,2,2,2,2,2,2,2,2,2,2,2,2,2,2,2,4),(59.7873029751542,
59.8213176769373,59.9851463211867,60.1455275333865,60.3029742107817,60.4678429536221,
60.6264020880418,60.7878657484224,60.9506812879062,61.107471377028,61.2712808583781,
61.4321876678488,61.5890773203166,61.7545218029967,61.913575824595,62.0736472442929,
62.2370285455998,62.3872680920556),.UNSPECIFIED.);
#955=B_SPLINE_CURVE_WITH_KNOTS('',3,(#27512,#27513,#27514,#27515,#27516,
#27517,#27518,#27519),.UNSPECIFIED.,.F.,.F.,(4,2,2,4),(64.9871389669336,
65.1296711980224,65.2172690762215,65.3048855506376),.UNSPECIFIED.);
#956=B_SPLINE_CURVE_WITH_KNOTS('',3,(#27522,#27523,#27524,#27525,#27526,
#27527,#27528,#27529,#27530,#27531,#27532,#27533,#27534,#27535,#27536,#27537),
 .UNSPECIFIED.,.F.,.F.,(4,2,2,2,2,2,2,4),(0.,0.0888555353420051,0.177236701399272,
0.337381099353558,0.501224862287476,0.657691166279862,0.819680858070591,
0.975100065405521),.UNSPECIFIED.);
#957=B_SPLINE_CURVE_WITH_KNOTS('',3,(#27550,#27551,#27552,#27553,#27554,
#27555,#27556,#27557,#27558,#27559,#27560,#27561,#27562,#27563,#27564,#27565,
#27566,#27567,#27568,#27569,#27570,#27571,#27572,#27573,#27574,#27575,#27576,
#27577,#27578,#27579,#27580,#27581,#27582,#27583),.UNSPECIFIED.,.F.,.F.,
(4,2,2,2,2,2,2,2,2,2,2,2,2,2,2,2,4),(0.,0.0200190791396383,0.0342447058880318,
0.0622704019494858,0.138479246631928,0.207804595812129,0.31343546609501,
0.445646771066455,0.604311883207654,0.806831895759981,1.16880638589577,
1.2714352086145,1.35107618267665,1.37963884460666,1.40478661373671,1.44768560678447,
1.58331119056091),.UNSPECIFIED.);
#958=B_SPLINE_CURVE_WITH_KNOTS('',3,(#27592,#27593,#27594,#27595,#27596,
#27597,#27598,#27599,#27600,#27601,#27602,#27603,#27604,#27605,#27606,#27607,
#27608,#27609,#27610,#27611,#27612,#27613,#27614,#27615,#27616,#27617,#27618,
#27619,#27620,#27621,#27622,#27623,#27624,#27625),.UNSPECIFIED.,.F.,.F.,
(4,2,2,2,2,2,2,2,2,2,2,2,2,2,2,2,4),(0.,0.0200190791268279,0.0342447058137099,
0.062270401610795,0.138479245078895,0.207804592960761,0.313435460954431,
0.445646763082409,0.604311871816074,0.806831880422644,1.168806362678,1.27143518292978,
1.35107615505061,1.37963881630498,1.40478658485205,1.44768557691437,1.58331115935392),
 .UNSPECIFIED.);
#959=B_SPLINE_CURVE_WITH_KNOTS('',3,(#27641,#27642,#27643,#27644,#27645,
#27646,#27647,#27648,#27649,#27650,#27651,#27652,#27653,#27654,#27655,#27656,
#27657,#27658,#27659,#27660,#27661,#27662,#27663,#27664,#27665,#27666,#27667,
#27668,#27669,#27670,#27671,#27672,#27673,#27674,#27675,#27676,#27677,#27678,
#27679,#27680,#27681,#27682,#27683,#27684,#27685,#27686,#27687,#27688,#27689,
#27690,#27691,#27692,#27693,#27694,#27695,#27696,#27697,#27698,#27699,#27700,
#27701,#27702,#27703,#27704,#27705,#27706,#27707,#27708,#27709,#27710,#27711,
#27712,#27713,#27714,#27715,#27716,#27717,#27718,#27719,#27720,#27721,#27722,
#27723,#27724,#27725,#27726,#27727,#27728,#27729,#27730,#27731,#27732,#27733,
#27734,#27735,#27736,#27737,#27738,#27739,#27740,#27741,#27742,#27743,#27744,
#27745,#27746,#27747,#27748,#27749,#27750,#27751,#27752,#27753,#27754,#27755,
#27756,#27757,#27758,#27759,#27760,#27761,#27762,#27763,#27764,#27765,#27766,
#27767,#27768,#27769,#27770,#27771,#27772,#27773,#27774,#27775,#27776,#27777,
#27778,#27779,#27780,#27781,#27782,#27783,#27784,#27785,#27786,#27787,#27788,
#27789,#27790,#27791,#27792,#27793,#27794,#27795,#27796,#27797,#27798,#27799,
#27800,#27801,#27802,#27803,#27804,#27805,#27806,#27807,#27808,#27809,#27810,
#27811,#27812),.UNSPECIFIED.,.F.,.F.,(4,3,3,3,3,3,3,3,3,3,3,3,3,3,3,3,3,
3,3,3,3,3,3,3,3,3,3,3,3,3,3,3,3,3,3,3,3,3,3,3,3,3,3,3,3,3,3,3,3,3,3,3,3,
3,3,3,3,4),(0.,0.0123304528366813,0.015625,0.0234375,0.02734375,0.0301056900711975,
0.03125,0.046875,0.0546875,0.0594470156310227,0.0625,0.075247186070732,
0.088385422654067,0.09375,0.107364232132532,0.121140761267218,0.125,0.147800625991517,
0.171014013031671,0.1875,0.21875,0.25,0.291221604078999,0.330354604152427,
0.367655777317147,0.402706302973929,0.436731165753159,0.469340412865769,
0.5,0.532623098826544,0.565615945128827,0.599234685440434,0.625,0.66623935755091,
0.713840887684498,0.75,0.7738913879151,0.796705025179732,0.8125,0.84375,
0.857899936485349,0.871788138789888,0.875,0.888569347832588,0.902293044929379,
0.90625,0.921875,0.9296875,0.934420440289022,0.9375,0.953125,0.9609375,
0.96484375,0.967460263406796,0.96875,0.981091439099429,0.993421435631299,
1.),.UNSPECIFIED.);
#960=B_SPLINE_CURVE_WITH_KNOTS('',3,(#27819,#27820,#27821,#27822,#27823,
#27824,#27825,#27826,#27827,#27828,#27829,#27830,#27831,#27832,#27833,#27834,
#27835,#27836,#27837,#27838,#27839,#27840,#27841,#27842,#27843,#27844,#27845,
#27846,#27847,#27848,#27849,#27850,#27851,#27852,#27853,#27854,#27855,#27856,
#27857,#27858,#27859,#27860,#27861,#27862,#27863,#27864,#27865,#27866,#27867,
#27868,#27869,#27870,#27871,#27872,#27873,#27874,#27875,#27876,#27877,#27878,
#27879,#27880,#27881,#27882,#27883,#27884,#27885,#27886,#27887,#27888,#27889,
#27890,#27891,#27892,#27893,#27894,#27895,#27896,#27897,#27898,#27899,#27900,
#27901,#27902,#27903,#27904,#27905,#27906,#27907,#27908,#27909,#27910,#27911,
#27912,#27913,#27914,#27915,#27916,#27917,#27918,#27919,#27920,#27921,#27922,
#27923,#27924,#27925,#27926,#27927,#27928,#27929,#27930,#27931,#27932,#27933,
#27934,#27935,#27936,#27937,#27938,#27939,#27940,#27941,#27942,#27943,#27944,
#27945,#27946,#27947,#27948,#27949,#27950,#27951,#27952,#27953,#27954,#27955,
#27956,#27957,#27958,#27959,#27960,#27961,#27962,#27963,#27964,#27965,#27966,
#27967,#27968,#27969,#27970,#27971,#27972,#27973,#27974,#27975,#27976,#27977,
#27978,#27979,#27980,#27981,#27982,#27983,#27984,#27985,#27986,#27987,#27988,
#27989,#27990),.UNSPECIFIED.,.F.,.F.,(4,3,3,3,3,3,3,3,3,3,3,3,3,3,3,3,3,
3,3,3,3,3,3,3,3,3,3,3,3,3,3,3,3,3,3,3,3,3,3,3,3,3,3,3,3,3,3,3,3,3,3,3,3,
3,3,3,3,4),(0.,0.0123304529175167,0.015625,0.0234375,0.02734375,0.0301056900816795,
0.03125,0.0520631268126456,0.0546875,0.0594470156580883,0.0625,0.0752471860780028,
0.0883854226637524,0.09375,0.107364232235248,0.121140761476458,0.125,0.147800626053147,
0.171014013162799,0.1875,0.21875,0.25,0.291221604248134,0.33035460442656,
0.367655777650242,0.402706303325056,0.436731166106891,0.469340413207235,
0.5,0.532623098825363,0.565615945123432,0.599234685425392,0.625,0.666239357866276,
0.713840888882716,0.75,0.773891388313745,0.796705025965584,0.8125,0.84375,
0.857899936516628,0.871788138848581,0.875,0.888569347967903,0.902293045202129,
0.90625,0.921875,0.9296875,0.934420440304062,0.9375,0.953125,0.9609375,
0.96484375,0.967460263411401,0.96875,0.981091439135241,0.993421435702746,
1.),.UNSPECIFIED.);
#961=B_SPLINE_CURVE_WITH_KNOTS('',3,(#28009,#28010,#28011,#28012,#28013,
#28014,#28015,#28016,#28017,#28018,#28019,#28020,#28021,#28022,#28023,#28024,
#28025,#28026,#28027,#28028,#28029,#28030,#28031,#28032,#28033,#28034,#28035,
#28036,#28037,#28038,#28039,#28040,#28041,#28042,#28043,#28044,#28045,#28046),
 .UNSPECIFIED.,.F.,.F.,(4,2,2,2,2,2,2,2,2,2,2,2,2,2,2,2,2,2,4),(0.975100065405521,
0.983650720032818,1.14149968175405,1.30554854967722,1.4642415654359,1.6238861288094,
1.78774983079492,1.944297258767,2.10575797334962,2.26959209753089,2.42691864100778,
2.59037021955754,2.75029520673997,2.90941141310176,3.0749281527528,3.23177015259627,
3.39274353675959,3.5565536980093,3.57510705038708),.UNSPECIFIED.);
#962=B_SPLINE_CURVE_WITH_KNOTS('',3,(#28047,#28048,#28049,#28050,#28051,
#28052,#28053,#28054,#28055,#28056,#28057,#28058,#28059,#28060,#28061,#28062,
#28063,#28064,#28065,#28066,#28067,#28068,#28069,#28070,#28071,#28072,#28073,
#28074,#28075,#28076,#28077,#28078,#28079,#28080,#28081,#28082,#28083,#28084),
 .UNSPECIFIED.,.F.,.F.,(4,2,2,2,2,2,2,2,2,2,2,2,2,2,2,2,2,2,4),(62.3872680920556,
62.3942929217837,62.5581159138936,62.7195133790498,62.8760794400901,63.0399401958598,
63.1995242071887,63.3583274114545,63.5223087369075,63.6800983500538,63.8442771207718,
64.0061978767224,64.1626564560649,64.3264972909694,64.4865768024129,64.6444627786545,
64.8089977143487,64.9672684116498,64.9871389669336),.UNSPECIFIED.);
#963=B_SPLINE_CURVE_WITH_KNOTS('',3,(#28086,#28087,#28088,#28089,#28090,
#28091,#28092,#28093,#28094,#28095,#28096,#28097,#28098,#28099),
 .UNSPECIFIED.,.F.,.F.,(4,2,2,2,2,2,4),(-0.787689357170944,-0.679879919295326,
-0.568513455580561,-0.412331745472765,-0.251692020866062,-0.13048064500736,
0.),.UNSPECIFIED.);
#964=B_SPLINE_CURVE_WITH_KNOTS('',3,(#28100,#28101,#28102,#28103,#28104,
#28105,#28106,#28107,#28108,#28109,#28110,#28111,#28112,#28113),
 .UNSPECIFIED.,.F.,.F.,(4,2,2,2,2,2,4),(-0.921983674052104,-0.763174312937053,
-0.618141011889387,-0.428360064692964,-0.24740957459713,-0.123269265571007,
0.),.UNSPECIFIED.);
#965=B_SPLINE_CURVE_WITH_KNOTS('',3,(#30002,#30003,#30004,#30005,#30006,
#30007,#30008,#30009,#30010,#30011),.UNSPECIFIED.,.F.,.F.,(4,3,3,4),(9.57246758340288E-17,
0.000355403916957923,0.000707000583199714,0.00104888238406079),
 .UNSPECIFIED.);
#966=B_SPLINE_CURVE_WITH_KNOTS('',3,(#30015,#30016,#30017,#30018,#30019,
#30020,#30021,#30022,#30023,#30024),.UNSPECIFIED.,.F.,.F.,(4,3,3,4),(0.,
0.00035058235323811,0.000705441803886655,0.0010488823840608),
 .UNSPECIFIED.);
#967=B_SPLINE_CURVE_WITH_KNOTS('',3,(#30030,#30031,#30032,#30033,#30034,
#30035,#30036,#30037,#30038,#30039,#30040,#30041,#30042,#30043,#30044,#30045,
#30046,#30047,#30048,#30049,#30050,#30051,#30052,#30053,#30054,#30055,#30056,
#30057,#30058,#30059,#30060,#30061,#30062,#30063,#30064,#30065,#30066,#30067,
#30068,#30069,#30070,#30071,#30072,#30073,#30074,#30075,#30076,#30077,#30078,
#30079,#30080,#30081,#30082,#30083,#30084,#30085,#30086,#30087,#30088,#30089,
#30090,#30091,#30092,#30093,#30094,#30095,#30096),.UNSPECIFIED.,.F.,.F.,
(4,3,3,3,3,3,3,3,3,3,3,3,3,3,3,3,3,3,3,3,3,3,4),(1.12014731928769E-16,2.44686880794631E-5,
5.01962031411245E-5,6.46659802217382E-5,9.34320062910693E-5,0.000117250238179507,
0.0001221980323604,0.000160663500114897,0.000207281263733168,0.000216514808073292,
0.000286414601198953,0.000321327000229682,0.000388105160880686,0.000522741781205867,
0.000642654000459244,0.000713976475490795,0.000947916545100924,0.00121389085366499,
0.00128530800091837,0.0013411477040794,0.00178543654748138,0.00228581177424824,
0.00257061600183662),.UNSPECIFIED.);
#968=B_SPLINE_CURVE_WITH_KNOTS('',3,(#30097,#30098,#30099,#30100,#30101,
#30102,#30103,#30104,#30105,#30106,#30107,#30108,#30109,#30110,#30111,#30112,
#30113,#30114,#30115,#30116,#30117,#30118,#30119,#30120,#30121,#30122,#30123,
#30124,#30125,#30126,#30127,#30128,#30129,#30130,#30131,#30132,#30133,#30134,
#30135,#30136,#30137,#30138,#30139,#30140,#30141,#30142,#30143,#30144,#30145,
#30146,#30147,#30148,#30149,#30150,#30151,#30152,#30153,#30154,#30155,#30156,
#30157),.UNSPECIFIED.,.F.,.F.,(4,3,3,3,3,3,3,3,3,3,3,3,3,3,3,3,3,3,3,3,
4),(0.,0.00046515412756322,0.000882411108678421,0.0012173266037486,0.00127005672264322,
0.00158659639906562,0.00183772251820228,0.00190508508396483,0.00203713318246821,
0.00215739978931402,0.00222259926462564,0.00227522662628161,0.00232413118357583,
0.00232785398793758,0.00236109891842404,0.00238135635495604,0.00242717801579792,
0.00245270320014808,0.0024836859974019,0.00251622256417103,0.00254011344528644),
 .UNSPECIFIED.);
#969=B_SPLINE_CURVE_WITH_KNOTS('',3,(#30160,#30161,#30162,#30163,#30164,
#30165,#30166,#30167,#30168,#30169,#30170,#30171,#30172,#30173,#30174,#30175,
#30176,#30177,#30178,#30179,#30180,#30181,#30182,#30183,#30184,#30185,#30186,
#30187,#30188,#30189,#30190,#30191,#30192,#30193,#30194,#30195,#30196,#30197,
#30198,#30199,#30200,#30201,#30202,#30203,#30204,#30205,#30206,#30207,#30208,
#30209,#30210,#30211,#30212,#30213,#30214,#30215,#30216,#30217,#30218,#30219,
#30220,#30221,#30222,#30223,#30224,#30225,#30226),.UNSPECIFIED.,.F.,.F.,
(4,3,3,3,3,3,3,3,3,3,3,3,3,3,3,3,3,3,3,3,3,3,4),(6.34356547860961E-12,2.91015092365536E-5,
2.91145195680595E-5,5.82134784524454E-5,5.8229039136119E-5,0.000116442640098838,
0.000116458078272238,0.000232900963425353,0.000232916156544486,0.000465817610066878,
0.000465832313088972,0.000931650903358755,0.000931664626177945,0.0018633174899382,
0.00186332925235589,0.00372665066309962,0.00372665850471178,0.00465831724968086,
0.00465832313088973,0.0055899838362617,0.00558998775706768,0.00723192026679969,
0.00745331700942357),.UNSPECIFIED.);
#970=B_SPLINE_CURVE_WITH_KNOTS('',3,(#30228,#30229,#30230,#30231,#30232,
#30233,#30234,#30235,#30236,#30237,#30238,#30239,#30240,#30241,#30242,#30243,
#30244,#30245,#30246,#30247,#30248,#30249,#30250,#30251,#30252,#30253,#30254,
#30255,#30256,#30257,#30258,#30259,#30260,#30261,#30262,#30263,#30264,#30265,
#30266,#30267,#30268,#30269,#30270,#30271,#30272,#30273,#30274,#30275,#30276,
#30277,#30278,#30279,#30280,#30281,#30282,#30283,#30284,#30285,#30286,#30287,
#30288,#30289,#30290,#30291,#30292,#30293,#30294),.UNSPECIFIED.,.F.,.F.,
(4,3,3,3,3,3,3,3,3,3,3,3,3,3,3,3,3,3,3,3,3,3,4),(4.33816373096554E-18,0.00158697662988317,
0.00180096318079261,0.00180096697037075,0.00270144477118891,0.0027014504555561,
0.00360192636158522,0.00360193394074181,0.00540288954237782,0.00540290091111227,
0.00630337113277412,0.00630338439629625,0.00675361192797227,0.00675362613889033,
0.00697873232557134,0.0069787470101831,0.00709129252437088,0.00709130744503989,
0.00714757262377064,0.00714758767823208,0.00717571267347053,0.00717572524835171,
0.00719063527707478),.UNSPECIFIED.);
#971=B_SPLINE_CURVE_WITH_KNOTS('',3,(#30298,#30299,#30300,#30301),
 .UNSPECIFIED.,.F.,.F.,(4,4),(0.00719063527707478,0.00720385271268794),
 .UNSPECIFIED.);
#972=B_SPLINE_CURVE_WITH_KNOTS('',3,(#30310,#30311,#30312,#30313,#30314,
#30315,#30316,#30317,#30318,#30319,#30320,#30321,#30322,#30323,#30324,#30325,
#30326,#30327,#30328,#30329,#30330,#30331,#30332,#30333,#30334,#30335,#30336,
#30337,#30338,#30339,#30340,#30341,#30342,#30343,#30344,#30345,#30346,#30347,
#30348,#30349,#30350,#30351,#30352,#30353,#30354,#30355,#30356,#30357,#30358,
#30359,#30360,#30361,#30362,#30363,#30364,#30365,#30366,#30367,#30368,#30369,
#30370,#30371,#30372,#30373,#30374,#30375,#30376,#30377,#30378,#30379,#30380,
#30381,#30382,#30383,#30384,#30385,#30386,#30387,#30388,#30389,#30390,#30391,
#30392,#30393,#30394,#30395,#30396,#30397,#30398,#30399,#30400,#30401,#30402,
#30403,#30404,#30405,#30406,#30407,#30408,#30409,#30410,#30411,#30412,#30413,
#30414,#30415,#30416,#30417,#30418,#30419,#30420,#30421,#30422,#30423,#30424,
#30425,#30426,#30427,#30428,#30429,#30430,#30431,#30432,#30433,#30434,#30435,
#30436),.UNSPECIFIED.,.F.,.F.,(4,3,3,3,3,3,3,3,3,3,3,3,3,3,3,3,3,3,3,3,
3,3,3,3,3,3,3,3,3,3,3,3,3,3,3,3,3,3,3,3,3,3,4),(0.0187104358930852,0.0198797262251292,
0.0199481217388706,0.0207658399883224,0.0210490165571731,0.021186081177019,
0.0227741969642194,0.0233875972212611,0.0236455138385063,0.0244983758541658,
0.024556887553305,0.0254911534667947,0.025726177885349,0.0260776320456601,
0.026895468217393,0.0272825913183847,0.0278847304061735,0.028064758549437,
0.0284807962042684,0.0294503982294847,0.0296719241460166,0.0304033392135249,
0.0308553085637769,0.0315726295455689,0.0320297867900004,0.032682244583055,
0.0327419198776128,0.0331939007038932,0.0337336131064912,0.0337714568809753,
0.0339112102096568,0.034345218787789,0.0349152553128406,0.0350805005417007,
0.0354825389403645,0.0356651457077227,0.0359067035564612,0.0360469991704175,
0.0362497908737447,0.0366116523092686,0.0370487581095643,0.0371780544079827,
0.0374190812057887),.UNSPECIFIED.);
#973=B_SPLINE_CURVE_WITH_KNOTS('',3,(#30438,#30439,#30440,#30441,#30442,
#30443),.UNSPECIFIED.,.F.,.F.,(4,2,4),(-0.00187765892693451,-0.00093532678058844,
-6.51826565449196E-7),.UNSPECIFIED.);
#974=B_SPLINE_CURVE_WITH_KNOTS('',3,(#30451,#30452,#30453,#30454,#30455,
#30456,#30457,#30458,#30459,#30460,#30461,#30462,#30463,#30464,#30465,#30466,
#30467,#30468,#30469,#30470,#30471,#30472,#30473,#30474,#30475,#30476,#30477,
#30478,#30479,#30480,#30481,#30482,#30483,#30484,#30485,#30486,#30487,#30488,
#30489,#30490,#30491,#30492,#30493,#30494,#30495,#30496,#30497,#30498,#30499,
#30500,#30501,#30502,#30503,#30504,#30505,#30506,#30507,#30508,#30509,#30510,
#30511,#30512,#30513,#30514,#30515,#30516,#30517,#30518,#30519,#30520,#30521,
#30522,#30523,#30524,#30525,#30526,#30527,#30528,#30529,#30530,#30531,#30532,
#30533,#30534,#30535,#30536,#30537,#30538,#30539,#30540,#30541,#30542,#30543,
#30544,#30545,#30546,#30547,#30548,#30549,#30550,#30551,#30552,#30553,#30554,
#30555,#30556,#30557,#30558,#30559,#30560,#30561,#30562,#30563,#30564,#30565,
#30566,#30567,#30568,#30569,#30570,#30571,#30572,#30573,#30574,#30575,#30576,
#30577,#30578,#30579,#30580,#30581,#30582,#30583,#30584,#30585,#30586,#30587,
#30588,#30589,#30590,#30591,#30592),.UNSPECIFIED.,.F.,.F.,(4,3,3,3,3,3,
3,3,3,3,3,3,3,3,3,3,3,3,3,3,3,3,3,3,3,3,3,3,3,3,3,3,3,3,3,3,3,3,3,3,3,3,
3,3,3,3,3,4),(1.4149286155699E-6,0.00024128475743038,0.000632178371154065,
0.000806980085871294,0.00117072873889494,0.00137185559650634,0.00175538564403461,
0.00193588458492275,0.00229633258208871,0.00234004254917429,0.00250284011366328,
0.00292469945431397,0.00307277910263342,0.00345879313729314,0.00350935635945365,
0.00364629450818616,0.00422381295371362,0.004678670169733,0.00533094003789352,
0.00538807166103802,0.00606788887869631,0.00656252330787629,0.00701729779029169,
0.00774578828639105,0.0088092112391015,0.0089367826515657,0.00935592541085039,
0.0101349902304355,0.0105252392211297,0.0112073453952734,0.0113400647033204,
0.0116945530314091,0.0125954135092807,0.0134677368138639,0.0137717393674888,
0.0140331806519678,0.0146914487977971,0.0149985613295519,0.0152024944622471,
0.0162308220365952,0.0163718082725265,0.016968388316562,0.0174681862798869,
0.0175411220828058,0.0180728185856757,0.0186062516405492,0.0187085025636743,
0.0187104358930852),.UNSPECIFIED.);
#975=B_SPLINE_CURVE_WITH_KNOTS('',3,(#30596,#30597,#30598,#30599,#30600,
#30601,#30602,#30603,#30604,#30605,#30606,#30607,#30608,#30609),
 .UNSPECIFIED.,.F.,.F.,(4,2,2,2,2,2,4),(2.60208521396521E-18,0.00261973771586097,
0.00392960657379145,0.00523947543172193,0.00654934428965241,0.00785921314758289,
0.0104789508634439),.UNSPECIFIED.);
#976=B_SPLINE_CURVE_WITH_KNOTS('',3,(#30611,#30612,#30613,#30614,#30615,
#30616,#30617,#30618,#30619,#30620,#30621,#30622,#30623,#30624),
 .UNSPECIFIED.,.F.,.F.,(4,2,2,2,2,2,4),(6.14713909703637E-8,0.00263335930455818,
0.00395003895683728,0.00526671860911637,0.00658339826139546,0.00790007791367455,
0.0105334372182327),.UNSPECIFIED.);
#977=B_SPLINE_CURVE_WITH_KNOTS('',3,(#30630,#30631,#30632,#30633,#30634,
#30635,#30636,#30637,#30638,#30639),.UNSPECIFIED.,.F.,.F.,(4,2,2,2,4),(0.,
0.23587669570582,0.471753391411641,0.705378949636768,0.939004507861895),
 .UNSPECIFIED.);
#978=B_SPLINE_CURVE_WITH_KNOTS('',3,(#30644,#30645,#30646,#30647,#30648,
#30649,#30650,#30651,#30652,#30653),.UNSPECIFIED.,.F.,.F.,(4,2,2,2,4),(0.939004507861895,
1.17263006608702,1.40625562431215,1.64213232001797,1.87800901572379),
 .UNSPECIFIED.);
#979=B_SPLINE_CURVE_WITH_KNOTS('',3,(#30662,#30663,#30664,#30665,#30666,
#30667,#30668,#30669,#30670,#30671,#30672,#30673,#30674,#30675,#30676,#30677,
#30678,#30679,#30680,#30681,#30682,#30683,#30684,#30685,#30686,#30687,#30688,
#30689,#30690,#30691,#30692,#30693,#30694,#30695,#30696,#30697,#30698,#30699,
#30700,#30701,#30702,#30703,#30704,#30705,#30706,#30707,#30708,#30709,#30710,
#30711,#30712,#30713,#30714,#30715,#30716,#30717,#30718,#30719,#30720,#30721,
#30722,#30723,#30724,#30725,#30726,#30727,#30728,#30729,#30730,#30731,#30732,
#30733,#30734,#30735,#30736,#30737,#30738,#30739,#30740),.UNSPECIFIED.,
 .F.,.F.,(4,3,3,3,3,3,3,3,3,3,3,3,3,3,3,3,3,3,3,3,3,3,3,3,3,3,4),(1.48114181800469E-12,
1.62713353573857E-5,2.85253456785481E-5,2.91748611457617E-5,3.0602416023118E-5,
5.19981524978168E-5,5.83497222915234E-5,6.03636063786387E-5,0.000116699444583057,
0.000119109456676927,0.000233398889166133,0.000236199927572212,0.000466797778332297,
0.000469925964041112,0.000933595556664625,0.000936857543433071,0.00186719111332928,
0.00187024522129993,0.00362565651164336,0.00373438222665858,0.00373660042866314,
0.00466797778332323,0.00466967995109927,0.00560157333998787,0.00560272875185939,
0.00726089770434782,0.00746876445331715),.UNSPECIFIED.);
#980=B_SPLINE_CURVE_WITH_KNOTS('',3,(#30742,#30743,#30744,#30745,#30746,
#30747,#30748,#30749,#30750,#30751,#30752,#30753,#30754,#30755,#30756,#30757),
 .UNSPECIFIED.,.F.,.F.,(4,2,2,2,2,2,2,4),(0.,3.69926380493027E-5,7.39852760986054E-5,
0.000147970552197207,0.000295941104394409,0.000591882208788816,0.00118376441757763,
0.00236752883515526),.UNSPECIFIED.);
#981=B_SPLINE_CURVE_WITH_KNOTS('',3,(#30759,#30760,#30761,#30762,#30763,
#30764,#30765),.UNSPECIFIED.,.F.,.F.,(4,3,4),(0.,0.000624637568767089,0.00116946841139767),
 .UNSPECIFIED.);
#982=B_SPLINE_CURVE_WITH_KNOTS('',3,(#30769,#30770,#30771,#30772,#30773,
#30774,#30775,#30776,#30777,#30778,#30779,#30780,#30781,#30782),
 .UNSPECIFIED.,.F.,.F.,(4,2,2,2,2,2,4),(0.,0.00215799408414667,0.00323699112622001,
0.00431598816829334,0.00539498521036668,0.00647398225244002,0.00863197633658669),
 .UNSPECIFIED.);
#983=B_SPLINE_CURVE_WITH_KNOTS('',3,(#30784,#30785,#30786,#30787,#30788,
#30789,#30790,#30791,#30792,#30793,#30794,#30795,#30796,#30797,#30798,#30799,
#30800,#30801,#30802,#30803,#30804,#30805,#30806,#30807,#30808,#30809,#30810,
#30811,#30812,#30813,#30814,#30815,#30816,#30817,#30818,#30819,#30820,#30821,
#30822,#30823,#30824,#30825,#30826,#30827,#30828,#30829,#30830,#30831,#30832,
#30833,#30834,#30835,#30836,#30837,#30838,#30839,#30840,#30841,#30842,#30843,
#30844,#30845,#30846,#30847,#30848,#30849,#30850,#30851,#30852,#30853,#30854,
#30855,#30856,#30857,#30858,#30859,#30860,#30861,#30862,#30863,#30864,#30865,
#30866,#30867,#30868,#30869,#30870,#30871,#30872,#30873,#30874,#30875,#30876,
#30877,#30878,#30879,#30880,#30881,#30882,#30883,#30884,#30885,#30886,#30887,
#30888,#30889,#30890,#30891,#30892,#30893,#30894,#30895,#30896,#30897,#30898,
#30899,#30900,#30901,#30902,#30903,#30904,#30905,#30906,#30907,#30908,#30909,
#30910,#30911,#30912,#30913,#30914,#30915,#30916,#30917,#30918,#30919,#30920,
#30921,#30922,#30923,#30924,#30925,#30926,#30927,#30928,#30929,#30930,#30931,
#30932,#30933,#30934,#30935,#30936,#30937,#30938,#30939,#30940,#30941,#30942,
#30943,#30944,#30945,#30946,#30947,#30948,#30949,#30950,#30951,#30952,#30953,
#30954,#30955,#30956,#30957,#30958,#30959,#30960,#30961,#30962,#30963,#30964,
#30965,#30966,#30967,#30968,#30969,#30970,#30971,#30972,#30973,#30974,#30975,
#30976,#30977,#30978,#30979,#30980,#30981,#30982,#30983,#30984,#30985,#30986,
#30987,#30988,#30989,#30990,#30991,#30992,#30993,#30994,#30995,#30996,#30997,
#30998,#30999,#31000,#31001,#31002,#31003,#31004,#31005,#31006,#31007,#31008,
#31009,#31010,#31011,#31012,#31013,#31014,#31015,#31016,#31017,#31018,#31019,
#31020,#31021,#31022,#31023,#31024,#31025,#31026,#31027),.UNSPECIFIED.,
 .F.,.F.,(4,3,3,3,3,3,3,3,3,3,3,3,3,3,3,3,3,3,3,3,3,3,3,3,3,3,3,3,3,3,3,
3,3,3,3,3,3,3,3,3,3,3,3,3,3,3,3,3,3,3,3,3,3,3,3,3,3,3,3,3,3,3,3,3,3,3,3,
3,3,3,3,3,3,3,3,3,3,3,3,3,3,4),(6.64190588068549E-10,0.00015883717919967,
0.000661562575487372,0.000994806103415245,0.00116260554575537,0.00138085520112917,
0.00149220915512287,0.00166326601977262,0.00198961220683049,0.00216588071655761,
0.00267030663113129,0.00298441831024573,0.00317737089357229,0.00368692950170913,
0.00397922441366098,0.00458731308453751,0.00471140773606946,0.00497403051707622,
0.00573980998888102,0.00596883662049147,0.00676961605918934,0.00779952990691134,
0.00795844882732194,0.008643398393127,0.0088280406155012,0.00895325493073719,
0.00985354333845186,0.00994806103415243,0.010673080413176,0.0113658404477328,
0.011891944708529,0.0119376732409829,0.0126851783449462,0.013408573202733,
0.0139116067056583,0.0139272854478134,0.0144550918417944,0.0149150434308082,
0.0149220915512286,0.0159168976546438,0.0159173041609428,0.0165518344898443,
0.0169117037580591,0.0169188369330008,0.0176391579183572,0.0179065098614743,
0.0179228529559086,0.0189013159648895,0.0189308538029226,0.0195006539338095,
0.0198961220683048,0.0199428610575756,0.0209581619462027,0.0218857342751353,
0.0219816750595829,0.0226544548355501,0.0228805403785505,0.0230073178663708,
0.0237710581938644,0.0238753464819657,0.0240355283687645,0.0250012828336967,
0.0250653536857579,0.0258649586887962,0.0260955990941479,0.026789820669263,
0.0271245982346018,0.0277221457004299,0.0278545708956267,0.0281492510550362,
0.028658852638223,0.0288493769990419,0.0291659944242556,0.0296702290396597,
0.0298441831024571,0.0301723844621069,0.0305140708508808,0.0306728710844153,
0.0308389892058724,0.0311737826503289,0.031675697204179,0.0318337953069872),
 .UNSPECIFIED.);
#984=B_SPLINE_CURVE_WITH_KNOTS('',3,(#31029,#31030,#31031,#31032,#31033,
#31034,#31035,#31036,#31037,#31038,#31039,#31040,#31041,#31042),
 .UNSPECIFIED.,.F.,.F.,(4,2,2,2,2,2,4),(0.,0.00217004055772761,0.00325506083659142,
0.00434008111545523,0.00542510139431905,0.00651012167318285,0.00868016223091047),
 .UNSPECIFIED.);
#985=B_SPLINE_CURVE_WITH_KNOTS('',3,(#31046,#31047,#31048,#31049,#31050,
#31051,#31052),.UNSPECIFIED.,.F.,.F.,(4,3,4),(1.93947980722443E-18,0.000624637568797489,
0.00116946841139767),.UNSPECIFIED.);
#986=B_SPLINE_CURVE_WITH_KNOTS('',3,(#31054,#31055,#31056,#31057,#31058,
#31059,#31060,#31061,#31062,#31063,#31064,#31065,#31066,#31067,#31068,#31069,
#31070,#31071,#31072,#31073,#31074,#31075,#31076,#31077,#31078,#31079,#31080,
#31081,#31082,#31083,#31084,#31085,#31086,#31087,#31088,#31089,#31090,#31091,
#31092,#31093,#31094,#31095,#31096,#31097,#31098,#31099,#31100,#31101,#31102,
#31103,#31104,#31105,#31106,#31107,#31108,#31109,#31110,#31111,#31112,#31113,
#31114,#31115,#31116,#31117,#31118,#31119,#31120,#31121,#31122,#31123,#31124,
#31125,#31126,#31127,#31128,#31129,#31130,#31131,#31132,#31133,#31134,#31135,
#31136,#31137,#31138,#31139,#31140,#31141,#31142,#31143,#31144,#31145,#31146,
#31147,#31148,#31149,#31150,#31151,#31152,#31153,#31154,#31155,#31156),
 .UNSPECIFIED.,.F.,.F.,(4,3,3,3,3,3,3,3,3,3,3,3,3,3,3,3,3,3,3,3,3,3,3,3,
3,3,3,3,3,3,3,3,3,3,4),(0.,0.000848753575416885,0.00118770142037617,0.00118810169232347,
0.00178155213056426,0.00178416675818213,0.00193001480811129,0.00207847748565831,
0.00208223092752585,0.00215270882443182,0.00218982449381858,0.00222694016320533,
0.0022307594594149,0.00224549799789871,0.00225245718590873,0.00227681434394379,
0.00228899292296132,0.0022920375677157,0.00230117150197885,0.00230441261012628,
0.00231045041932553,0.00231219021632804,0.00231300574617296,0.00231379579071023,
0.00232604148103792,0.00233216432620176,0.00233369503749272,0.00233426905422683,
0.0023382871713656,0.00234060924917293,0.00234756608871229,0.00234843598721354,
0.00234927870138663,0.00236769555909942,0.00237540284075236),
 .UNSPECIFIED.);
#987=B_SPLINE_CURVE_WITH_KNOTS('',3,(#31157,#31158,#31159,#31160,#31161,
#31162,#31163,#31164,#31165,#31166,#31167,#31168,#31169,#31170,#31171,#31172,
#31173,#31174,#31175,#31176,#31177,#31178,#31179,#31180,#31181,#31182,#31183,
#31184,#31185,#31186,#31187,#31188,#31189,#31190,#31191,#31192,#31193,#31194,
#31195,#31196,#31197,#31198,#31199,#31200,#31201,#31202,#31203,#31204,#31205,
#31206,#31207,#31208,#31209,#31210,#31211,#31212,#31213,#31214,#31215,#31216,
#31217,#31218,#31219,#31220,#31221,#31222,#31223,#31224,#31225,#31226,#31227,
#31228,#31229,#31230,#31231,#31232,#31233,#31234,#31235),.UNSPECIFIED.,
 .F.,.F.,(4,3,3,3,3,3,3,3,3,3,3,3,3,3,3,3,3,3,3,3,3,3,3,3,3,3,4),(0.,0.00160045154295414,
0.00180108286976027,0.00180219806414393,0.00270165417736523,0.00270329709621589,
0.00360225513728841,0.00360439612828786,0.0052987050646637,0.00540364639161632,
0.00540659419243178,0.00630457583191594,0.00630769322450373,0.00675524744892423,
0.00675824274053971,0.00698081395851806,0.0069835174985577,0.00709382875298428,
0.00709615487756669,0.00715056271684698,0.00715247356707119,0.00717033207045985,
0.00717923745439373,0.00718063291182344,0.00719131802773085,0.00720628339444832,
0.00720879225482352),.UNSPECIFIED.);
#988=B_SPLINE_CURVE_WITH_KNOTS('',3,(#31442,#31443,#31444,#31445,#31446,
#31447,#31448,#31449,#31450,#31451,#31452,#31453,#31454,#31455,#31456,#31457,
#31458,#31459,#31460,#31461,#31462,#31463,#31464,#31465,#31466,#31467,#31468,
#31469,#31470,#31471,#31472,#31473,#31474,#31475,#31476,#31477,#31478,#31479,
#31480,#31481,#31482,#31483,#31484,#31485,#31486,#31487,#31488,#31489,#31490,
#31491,#31492,#31493,#31494,#31495,#31496,#31497,#31498,#31499,#31500,#31501,
#31502,#31503,#31504,#31505,#31506,#31507,#31508,#31509,#31510,#31511,#31512,
#31513,#31514,#31515,#31516,#31517),.UNSPECIFIED.,.F.,.F.,(4,3,3,3,3,3,
3,3,3,3,3,3,3,3,3,3,3,3,3,3,3,3,3,3,3,4),(1.92266797596103E-13,0.000100765253400692,
0.000203257746196736,0.000307659288333143,0.000415034136597425,0.000522822845455063,
0.000628818251273869,0.000674714477361159,0.000796110490146888,0.000926752228731723,
0.00108084544056301,0.00125483099502789,0.00134942895472221,0.00150980300002335,
0.0016863707781532,0.00182669577876767,0.00195048914404132,0.00202414343208326,
0.00212087565257403,0.00221840926324827,0.00231581884120266,0.00236150067076378,
0.00246857997997598,0.00257529118717096,0.00268062322103986,0.00269885790944431),
 .UNSPECIFIED.);
#989=B_SPLINE_CURVE_WITH_KNOTS('',3,(#31746,#31747,#31748,#31749,#31750,
#31751,#31752,#31753,#31754,#31755,#31756,#31757,#31758,#31759,#31760,#31761,
#31762,#31763,#31764,#31765,#31766,#31767,#31768,#31769,#31770,#31771,#31772,
#31773,#31774,#31775,#31776,#31777,#31778,#31779,#31780,#31781,#31782,#31783,
#31784,#31785,#31786,#31787,#31788,#31789,#31790,#31791,#31792,#31793,#31794,
#31795,#31796,#31797,#31798,#31799,#31800,#31801,#31802,#31803,#31804,#31805,
#31806,#31807,#31808,#31809,#31810,#31811,#31812,#31813,#31814,#31815,#31816,
#31817,#31818,#31819,#31820,#31821),.UNSPECIFIED.,.F.,.F.,(4,3,3,3,3,3,
3,3,3,3,3,3,3,3,3,3,3,3,3,3,3,3,3,3,3,4),(6.6900740202938E-10,0.000100568281496774,
0.000202839043311474,0.000306975484988691,0.000413993960739299,0.000521383938195942,
0.000626986625570161,0.000674714477360893,0.000795619140822781,0.000925351564806097,
0.00108316358964099,0.00125449955005232,0.0013494289547216,0.00150400641422797,
0.00167742957890143,0.0018187480346269,0.00194314871130111,0.00202414343208231,
0.00212118997393239,0.002219037980227,0.00231672327406803,0.00236150067076266,
0.00246941783078403,0.00257682685345429,0.00268261453841891,0.00269885790944302),
 .UNSPECIFIED.);
#990=B_SPLINE_CURVE_WITH_KNOTS('',3,(#32041,#32042,#32043,#32044),
 .UNSPECIFIED.,.F.,.F.,(4,4),(-0.193908494403496,-0.18144780310173),
 .UNSPECIFIED.);
#991=B_SPLINE_CURVE_WITH_KNOTS('',3,(#32046,#32047,#32048,#32049,#32050,
#32051,#32052,#32053,#32054,#32055,#32056,#32057,#32058,#32059,#32060,#32061,
#32062,#32063,#32064,#32065),.UNSPECIFIED.,.F.,.F.,(4,2,2,2,2,2,2,2,2,4),
(-0.167340420633072,-0.166972617746829,-0.154327111962806,-0.141796925934467,
-0.120672972956733,-0.101704261798647,-0.0839904703357835,-0.0660782047629785,
-0.0468280943861894,-0.0462066260650754),.UNSPECIFIED.);
#992=B_SPLINE_CURVE_WITH_KNOTS('',3,(#32071,#32072,#32073,#32074,#32075,
#32076,#32077,#32078),.UNSPECIFIED.,.F.,.F.,(4,2,2,4),(1.05683143574813,
1.07001373433151,1.09130065438089,1.09381163587351),.UNSPECIFIED.);
#993=B_SPLINE_CURVE_WITH_KNOTS('',3,(#32079,#32080,#32081,#32082,#32083,
#32084,#32085,#32086,#32087,#32088,#32089,#32090,#32091,#32092,#32093,#32094,
#32095,#32096,#32097,#32098,#32099,#32100,#32101,#32102,#32103,#32104,#32105,
#32106,#32107,#32108,#32109,#32110,#32111,#32112,#32113,#32114,#32115,#32116,
#32117,#32118,#32119,#32120,#32121,#32122,#32123,#32124,#32125,#32126,#32127,
#32128,#32129,#32130),.UNSPECIFIED.,.F.,.F.,(4,3,3,3,3,3,3,3,3,3,3,3,3,
3,3,3,3,4),(7.57505397569876E-13,9.10844499065638E-5,0.00018215489291624,
0.000272070717647245,0.000285322832162068,0.000352224089002271,0.00041905128827239,
0.000485831935717838,0.000552669909587165,0.000570645664324136,0.000642530907423814,
0.00071447615483413,0.000786742284179075,0.000855968496486203,0.00093427998969131,
0.00101288394362129,0.00109196298802677,0.00114129132864827),
 .UNSPECIFIED.);
#994=B_SPLINE_CURVE_WITH_KNOTS('',3,(#32140,#32141,#32142,#32143,#32144,
#32145,#32146,#32147,#32148,#32149,#32150,#32151,#32152,#32153,#32154,#32155,
#32156,#32157),.UNSPECIFIED.,.F.,.F.,(4,2,2,2,2,2,2,2,4),(-2.53894889799168,
-2.37885292235818,-2.21875694672469,-2.06148431010922,-1.90421167349376,
-1.7469390368783,-1.58966640026284,-1.42957042462934,-1.26947444899584),
 .UNSPECIFIED.);
#995=B_SPLINE_CURVE_WITH_KNOTS('',3,(#32161,#32162,#32163,#32164,#32165,
#32166,#32167,#32168,#32169,#32170,#32171,#32172,#32173,#32174,#32175,#32176,
#32177,#32178,#32179,#32180,#32181,#32182,#32183,#32184,#32185,#32186,#32187,
#32188,#32189,#32190,#32191,#32192,#32193,#32194,#32195,#32196,#32197,#32198,
#32199,#32200,#32201,#32202,#32203,#32204,#32205,#32206,#32207,#32208,#32209,
#32210,#32211,#32212,#32213,#32214,#32215,#32216,#32217,#32218,#32219,#32220,
#32221,#32222,#32223,#32224,#32225,#32226,#32227,#32228,#32229,#32230,#32231,
#32232,#32233,#32234,#32235,#32236,#32237,#32238,#32239,#32240,#32241,#32242,
#32243,#32244,#32245,#32246,#32247,#32248,#32249,#32250,#32251,#32252,#32253,
#32254,#32255,#32256,#32257,#32258,#32259,#32260,#32261,#32262,#32263,#32264,
#32265,#32266,#32267,#32268,#32269,#32270,#32271,#32272),.UNSPECIFIED.,
 .F.,.F.,(4,3,3,3,3,3,3,3,3,3,3,3,3,3,3,3,3,3,3,3,3,3,3,3,3,3,3,3,3,3,3,
3,3,3,3,3,3,4),(0.,0.000912210497134922,0.00137016845949825,0.0014036790570624,
0.00208601616582784,0.0021055185855936,0.00262363140207477,0.00279879558118489,
0.0028073581141248,0.00340274023561052,0.00350809265765975,0.003509197642656,
0.00395949408831714,0.0042110371711872,0.00421371707051397,0.00491287669971841,
0.00491670671448806,0.00528745106991125,0.00561471622824961,0.00561759561603492,
0.00631655575678081,0.00631897771198343,0.00671051133784849,0.00701839528531201,
0.00702163246524702,0.00772023481384321,0.00772763176352554,0.00824912212447548,
0.00842207434237441,0.00843697494939749,0.00902569097629585,0.00963836229883114,
0.00982575339943681,0.00986588374133253,0.0102491420369702,0.0106411882385985,
0.0110265915003307,0.0112294324564992),.UNSPECIFIED.);
#996=B_SPLINE_CURVE_WITH_KNOTS('',3,(#32284,#32285,#32286,#32287,#32288,
#32289,#32290,#32291,#32292,#32293,#32294,#32295,#32296,#32297,#32298,#32299,
#32300,#32301,#32302,#32303,#32304,#32305,#32306,#32307,#32308,#32309,#32310,
#32311,#32312,#32313,#32314,#32315,#32316,#32317,#32318,#32319,#32320,#32321,
#32322,#32323,#32324,#32325,#32326,#32327,#32328,#32329,#32330,#32331,#32332,
#32333,#32334,#32335,#32336,#32337,#32338,#32339,#32340,#32341,#32342,#32343,
#32344,#32345,#32346,#32347,#32348,#32349,#32350,#32351,#32352,#32353,#32354,
#32355,#32356,#32357,#32358,#32359,#32360,#32361,#32362,#32363,#32364,#32365,
#32366,#32367,#32368,#32369,#32370,#32371,#32372,#32373,#32374,#32375,#32376,
#32377,#32378,#32379,#32380),.UNSPECIFIED.,.F.,.F.,(4,3,3,3,3,3,3,3,3,3,
3,3,3,3,3,3,3,3,3,3,3,3,3,3,3,3,3,3,3,3,3,3,4),(0.,7.62914212120981E-5,
0.000184257247324592,0.000263187484407962,0.000292223073437087,0.00039911370766475,
0.000501087875789428,0.000584446146874173,0.00074654672592793,0.000907676866873101,
0.0010680512097945,0.00116889229374834,0.00140926922086005,0.00164595258360394,
0.00175333844062251,0.00197175143406078,0.0021842196106002,0.00233778458749668,
0.00254099318951238,0.0027343383349243,0.00292223073437084,0.00312940331866394,
0.00332978793388773,0.00350667688124501,0.00365713623155684,0.00380448204900645,
0.00394780253856282,0.00409112302811918,0.00423723456483772,0.00437340206388912,
0.00450594181348204,0.004633221785658,0.00467556917499335),
 .UNSPECIFIED.);
#997=B_SPLINE_CURVE_WITH_KNOTS('',3,(#32384,#32385,#32386,#32387,#32388,
#32389,#32390,#32391,#32392,#32393,#32394,#32395,#32396,#32397,#32398,#32399,
#32400,#32401,#32402,#32403,#32404,#32405,#32406,#32407,#32408,#32409,#32410,
#32411,#32412,#32413,#32414,#32415,#32416,#32417,#32418,#32419,#32420,#32421,
#32422,#32423,#32424,#32425,#32426,#32427,#32428,#32429,#32430,#32431,#32432,
#32433,#32434,#32435,#32436,#32437,#32438,#32439,#32440,#32441,#32442,#32443,
#32444,#32445,#32446,#32447,#32448,#32449,#32450,#32451,#32452,#32453,#32454,
#32455,#32456,#32457,#32458,#32459,#32460,#32461,#32462,#32463,#32464,#32465,
#32466,#32467,#32468,#32469,#32470,#32471,#32472,#32473,#32474,#32475,#32476,
#32477,#32478,#32479,#32480),.UNSPECIFIED.,.F.,.F.,(4,3,3,3,3,3,3,3,3,3,
3,3,3,3,3,3,3,3,3,3,3,3,3,3,3,3,3,3,3,3,3,3,4),(4.42269442734662E-18,0.00011510948078521,
0.000234103391159393,0.000285007760334435,0.000398078962146353,0.000512011060315604,
0.000570015520668867,0.000740289648794204,0.000914720697216612,0.001095344951612,
0.00114003104133773,0.00133186906084365,0.00152928739270689,0.00173576910686678,
0.00194759699451027,0.00216785204681413,0.00228006208267546,0.00249734619663865,
0.00272803292848229,0.00295230300576247,0.00318619806488783,0.00342009312401319,
0.00357729117862414,0.00373483837142073,0.0038935958084681,0.00399010864468205,
0.00408881194297815,0.00419123656775307,0.00427511640501648,0.00435284689245867,
0.00445648552890479,0.0045323946741616,0.00456012416535091),
 .UNSPECIFIED.);
#998=B_SPLINE_CURVE_WITH_KNOTS('',3,(#32499,#32500,#32501,#32502,#32503,
#32504,#32505,#32506),.UNSPECIFIED.,.F.,.F.,(4,2,2,4),(0.295121403805867,
0.297363449435658,0.307232092905955,0.311601659185375),.UNSPECIFIED.);
#999=B_SPLINE_CURVE_WITH_KNOTS('',3,(#32507,#32508,#32509,#32510,#32511,
#32512,#32513,#32514,#32515,#32516,#32517,#32518,#32519,#32520,#32521,#32522,
#32523,#32524,#32525,#32526,#32527,#32528,#32529,#32530,#32531,#32532),
 .UNSPECIFIED.,.F.,.F.,(4,2,2,2,2,2,2,2,2,2,2,2,4),(-7.41073495858817E-5,
0.00150429147127286,0.0030826902921316,0.00466108911299035,0.00545028852341972,
0.00623948793384909,0.00702868734427846,0.00781788675470783,0.0086070861651372,
0.00939628557556658,0.0101854849859959,0.0109746843964253,0.0125530832172841),
 .UNSPECIFIED.);
#1000=B_SPLINE_CURVE_WITH_KNOTS('',3,(#32549,#32550,#32551,#32552,#32553,
#32554,#32555,#32556,#32557,#32558,#32559,#32560,#32561,#32562,#32563,#32564,
#32565,#32566,#32567,#32568,#32569,#32570,#32571,#32572,#32573,#32574,#32575,
#32576,#32577,#32578,#32579,#32580,#32581,#32582,#32583,#32584,#32585,#32586,
#32587,#32588,#32589,#32590,#32591,#32592,#32593,#32594,#32595,#32596,#32597,
#32598,#32599,#32600,#32601,#32602,#32603,#32604,#32605,#32606),
 .UNSPECIFIED.,.F.,.F.,(4,3,3,3,3,3,3,3,3,3,3,3,3,3,3,3,3,3,3,4),(0.,0.000229129696581083,
0.000252698653230226,0.000253168160380289,0.000505898112004886,0.000506336320760579,
0.00101229703393971,0.00101267264152115,0.00202509487854447,0.00202534528304231,
0.00253149313182082,0.0030378927219851,0.00303801792456346,0.00329109194612974,
0.00354429164391778,0.00354435424532404,0.00379749110506874,0.00379752240570433,
0.00399904195215253,0.00405069056608462),.UNSPECIFIED.);
#1001=B_SPLINE_CURVE_WITH_KNOTS('',3,(#32610,#32611,#32612,#32613),
 .UNSPECIFIED.,.F.,.F.,(4,4),(-0.181459269355133,-0.168998578053366),
 .UNSPECIFIED.);
#1002=B_SPLINE_CURVE_WITH_KNOTS('',3,(#32617,#32618,#32619,#32620,#32621,
#32622,#32623,#32624,#32625,#32626,#32627,#32628,#32629,#32630,#32631,#32632,
#32633,#32634,#32635,#32636,#32637,#32638,#32639,#32640,#32641,#32642,#32643,
#32644,#32645,#32646,#32647,#32648,#32649,#32650,#32651,#32652,#32653,#32654,
#32655,#32656,#32657,#32658,#32659,#32660,#32661,#32662,#32663,#32664,#32665,
#32666,#32667,#32668,#32669,#32670,#32671,#32672,#32673,#32674,#32675,#32676,
#32677),.UNSPECIFIED.,.F.,.F.,(4,3,3,3,3,3,3,3,3,3,3,3,3,3,3,3,3,3,3,3,
4),(0.,0.000197327121899467,0.000247927056861424,0.000247930453861229,0.000495854113722848,
0.000495860907724086,0.000743791387463213,0.000991708227445701,0.000991721815445343,
0.00148758279649238,0.00198341645489141,0.00198344363088277,0.00297512468233711,
0.00297516544633371,0.00347097879605996,0.00347103971226963,0.00371890585292139,
0.00371913308887466,0.00381981107469357,0.0039024739051475,0.00396683290978282),
 .UNSPECIFIED.);
#1003=B_SPLINE_CURVE_WITH_KNOTS('',3,(#32751,#32752,#32753,#32754,#32755,
#32756,#32757,#32758,#32759,#32760,#32761,#32762,#32763,#32764,#32765,#32766,
#32767,#32768),.UNSPECIFIED.,.F.,.F.,(4,2,2,2,2,2,2,2,4),(-0.167140599481193,
-0.166773364806454,-0.146753267101867,-0.12714061423038,-0.106552389959774,
-0.0879503536354909,-0.0702956656303136,-0.0523482687226349,-0.0461614733531646),
 .UNSPECIFIED.);
#1004=B_SPLINE_CURVE_WITH_KNOTS('',3,(#32770,#32771,#32772,#32773,#32774,
#32775,#32776,#32777,#32778,#32779,#32780,#32781,#32782,#32783,#32784,#32785,
#32786,#32787,#32788,#32789,#32790,#32791,#32792,#32793,#32794,#32795,#32796,
#32797,#32798,#32799,#32800,#32801,#32802,#32803,#32804,#32805,#32806,#32807,
#32808,#32809,#32810,#32811,#32812,#32813,#32814,#32815,#32816,#32817,#32818,
#32819,#32820,#32821),.UNSPECIFIED.,.F.,.F.,(4,3,3,3,3,3,3,3,3,3,3,3,3,
3,3,3,3,4),(0.,9.10844491467422E-5,0.000182154892159899,0.000272070716897632,
0.000285322832163043,0.000352224089003363,0.000419051288273606,0.000485831935719175,
0.000552669909588621,0.000570645664326085,0.000642530907424901,0.000714476154834331,
0.000786742284178373,0.000855968496489128,0.000934279989732564,0.00101288394370409,
0.0010919629881535,0.00114129132865217),.UNSPECIFIED.);
#1005=B_SPLINE_CURVE_WITH_KNOTS('',3,(#33448,#33449,#33450,#33451,#33452,
#33453,#33454,#33455,#33456,#33457,#33458,#33459,#33460,#33461,#33462,#33463,
#33464,#33465,#33466,#33467,#33468,#33469,#33470,#33471,#33472,#33473,#33474),
 .UNSPECIFIED.,.F.,.F.,(4,2,2,2,2,2,3,2,2,2,2,2,4),(-0.332209547359341,
-0.298546270509129,-0.214461346284245,-0.130376422059361,-0.0858276476044183,
-0.0429138238022092,0.,0.0429138238022091,0.0858276476044183,0.130376422059361,
0.214461346284245,0.298546270509129,0.332209547359342),.UNSPECIFIED.);
#1006=B_SPLINE_CURVE_WITH_KNOTS('',3,(#33640,#33641,#33642,#33643),
 .UNSPECIFIED.,.F.,.F.,(4,4),(0.,0.000427835206687807),.UNSPECIFIED.);
#1007=B_SPLINE_CURVE_WITH_KNOTS('',3,(#33644,#33645,#33646,#33647),
 .UNSPECIFIED.,.F.,.F.,(4,4),(0.,0.000427835206687776),.UNSPECIFIED.);
#1008=B_SPLINE_CURVE_WITH_KNOTS('',3,(#33652,#33653,#33654,#33655),
 .UNSPECIFIED.,.F.,.F.,(4,4),(0.,0.000427835206687808),.UNSPECIFIED.);
#1009=B_SPLINE_CURVE_WITH_KNOTS('',3,(#33656,#33657,#33658,#33659),
 .UNSPECIFIED.,.F.,.F.,(4,4),(3.46944695195361E-18,0.000427835206687798),
 .UNSPECIFIED.);
#1010=B_SPLINE_CURVE_WITH_KNOTS('',3,(#33667,#33668,#33669,#33670),
 .UNSPECIFIED.,.F.,.F.,(4,4),(0.,0.000427835206687807),.UNSPECIFIED.);
#1011=B_SPLINE_CURVE_WITH_KNOTS('',3,(#33671,#33672,#33673,#33674),
 .UNSPECIFIED.,.F.,.F.,(4,4),(0.,0.000427835206687801),.UNSPECIFIED.);
#1012=B_SPLINE_CURVE_WITH_KNOTS('',3,(#33684,#33685,#33686,#33687),
 .UNSPECIFIED.,.F.,.F.,(4,4),(0.,0.000427835206687808),.UNSPECIFIED.);
#1013=B_SPLINE_CURVE_WITH_KNOTS('',3,(#33688,#33689,#33690,#33691),
 .UNSPECIFIED.,.F.,.F.,(4,4),(3.46944695195361E-18,0.000427835206687774),
 .UNSPECIFIED.);
#1014=B_SPLINE_CURVE_WITH_KNOTS('',3,(#36242,#36243,#36244,#36245,#36246,
#36247,#36248,#36249,#36250,#36251),.UNSPECIFIED.,.F.,.F.,(4,2,2,2,4),(0.407230824200947,
0.441482308570059,0.475169509556855,0.508523321203204,0.522738749128563),
 .UNSPECIFIED.);
#1015=B_SPLINE_CURVE_WITH_KNOTS('',3,(#36255,#36256,#36257,#36258,#36259,
#36260,#36261,#36262,#36263,#36264),.UNSPECIFIED.,.F.,.F.,(4,2,2,2,4),(0.0189522566102193,
0.0331676845355794,0.0665214961819283,0.100208697168724,0.134460181537836),
 .UNSPECIFIED.);
#1016=B_SPLINE_CURVE_WITH_KNOTS('',3,(#36275,#36276,#36277,#36278,#36279,
#36280,#36281,#36282,#36283,#36284),.UNSPECIFIED.,.F.,.F.,(4,2,2,2,4),(0.407230824200947,
0.441482308570059,0.475169509556855,0.508523321203204,0.522738749128564),
 .UNSPECIFIED.);
#1017=B_SPLINE_CURVE_WITH_KNOTS('',3,(#36287,#36288,#36289,#36290,#36291,
#36292,#36293,#36294,#36295,#36296),.UNSPECIFIED.,.F.,.F.,(4,2,2,2,4),(0.0189522566102211,
0.0331676845355794,0.0665214961819283,0.100208697168724,0.134460181537836),
 .UNSPECIFIED.);
#1018=CONICAL_SURFACE('',#17892,2.6,1.02974425867665);
#1019=CONICAL_SURFACE('',#17895,7.,0.785398163397448);
#1020=CONICAL_SURFACE('',#17898,8.69677462715879,0.916297857297022);
#1021=CONICAL_SURFACE('',#17904,10.,0.261799387799149);
#1022=CONICAL_SURFACE('',#17964,4.15,0.785398163397535);
#1023=CONICAL_SURFACE('',#18043,10.,0.785398163397448);
#1024=CONICAL_SURFACE('',#18048,4.,0.78539816339745);
#1025=CONICAL_SURFACE('',#18059,7.85653654166145,0.904103500540624);
#1026=CONICAL_SURFACE('',#18079,12.25,0.118705337143177);
#1027=CONICAL_SURFACE('',#18140,6.,0.0336517539394116);
#1028=CONICAL_SURFACE('',#18144,5.5,0.785398163397448);
#1029=CONICAL_SURFACE('',#18158,4.94835215326525,0.833377149502852);
#1030=CONICAL_SURFACE('',#18172,6.72023753462643,0.0479789861054062);
#1031=CONICAL_SURFACE('',#18209,4.,0.0465431041182806);
#1032=CONICAL_SURFACE('',#18213,3.5,0.785398163397448);
#1033=CONICAL_SURFACE('',#18224,4.25,0.643501108793284);
#1034=CONICAL_SURFACE('',#18230,5.,0.927295218001612);
#1035=CONICAL_SURFACE('',#18448,2.,0.785398163397458);
#1036=CONICAL_SURFACE('',#18451,1.80000000000002,0.785398163397445);
#1037=CONICAL_SURFACE('',#18455,2.3,0.785398163397448);
#1038=CONICAL_SURFACE('',#18459,1.2,0.785398163397454);
#1039=CONICAL_SURFACE('',#18462,3.49999999999998,0.78539816339745);
#1040=CONICAL_SURFACE('',#18465,1.50000000000001,0.785398163397452);
#1041=CONICAL_SURFACE('',#18469,2.3,0.785398163397444);
#1042=CONICAL_SURFACE('',#18473,2.,0.78539816339744);
#1043=CONICAL_SURFACE('',#18476,1.5,0.785398163397444);
#1044=CONICAL_SURFACE('',#18479,3.2,0.785398163397442);
#1045=CONICAL_SURFACE('',#18593,4.,0.785398163397445);
#1046=CONICAL_SURFACE('',#18594,4.,0.785398163397445);
#1047=CONICAL_SURFACE('',#18595,4.29999999999999,0.785398163397445);
#1048=CONICAL_SURFACE('',#18596,4.29999999999998,0.785398163397451);
#1049=CONICAL_SURFACE('',#18660,2.,0.785398163397446);
#1050=CONICAL_SURFACE('',#18664,1.61,0.959931088596875);
#1051=CONICAL_SURFACE('',#18669,2.,0.959931088596884);
#1052=CONICAL_SURFACE('',#18673,1.61,0.959931088596875);
#1053=CONICAL_SURFACE('',#18678,2.,0.959931088596884);
#1054=CONICAL_SURFACE('',#18682,1.61,0.959931088596875);
#1055=CONICAL_SURFACE('',#18687,2.,0.959931088596884);
#1056=CONICAL_SURFACE('',#18691,1.61,0.959931088596875);
#1057=CONICAL_SURFACE('',#18696,2.,0.959931088596884);
#1058=CONICAL_SURFACE('',#18700,1.61,0.959931088596875);
#1059=CONICAL_SURFACE('',#18705,2.,0.959931088596884);
#1060=CONICAL_SURFACE('',#18709,1.61,0.959931088596875);
#1061=CONICAL_SURFACE('',#18714,2.,0.959931088596884);
#1062=CONICAL_SURFACE('',#18718,1.61,0.959931088596875);
#1063=CONICAL_SURFACE('',#18723,2.,0.959931088596884);
#1064=CONICAL_SURFACE('',#18727,1.61,0.959931088596875);
#1065=CONICAL_SURFACE('',#18732,2.,0.959931088596884);
#1066=CONICAL_SURFACE('',#18736,1.61,0.959931088596875);
#1067=CONICAL_SURFACE('',#18741,2.,0.959931088596884);
#1068=CONICAL_SURFACE('',#18745,1.61,0.959931088596875);
#1069=CONICAL_SURFACE('',#18750,2.,0.959931088596884);
#1070=CONICAL_SURFACE('',#18754,1.61,0.959931088596875);
#1071=CONICAL_SURFACE('',#18759,2.,0.959931088596884);
#1072=CONICAL_SURFACE('',#18763,1.61,0.959931088596875);
#1073=CONICAL_SURFACE('',#18768,2.,0.959931088596884);
#1074=CONICAL_SURFACE('',#18772,1.61,0.959931088596875);
#1075=CONICAL_SURFACE('',#18777,2.,0.959931088596884);
#1076=CONICAL_SURFACE('',#18781,1.61,0.959931088596875);
#1077=CONICAL_SURFACE('',#18786,2.,0.959931088596884);
#1078=CONICAL_SURFACE('',#18790,1.61,0.959931088596875);
#1079=CONICAL_SURFACE('',#18795,2.,0.959931088596884);
#1080=CONICAL_SURFACE('',#18796,8.175,0.785398163397451);
#1081=CONICAL_SURFACE('',#18875,8.175,0.785398163397451);
#1082=CONICAL_SURFACE('',#19198,2.64252040565333,0.0872664625997168);
#1083=CONICAL_SURFACE('',#19214,2.,0.785398163397446);
#1084=CONICAL_SURFACE('',#19218,1.61,0.959931088596878);
#1085=CONICAL_SURFACE('',#19223,2.,0.959931088596884);
#1086=CONICAL_SURFACE('',#19227,1.61,0.959931088596878);
#1087=CONICAL_SURFACE('',#19232,2.,0.959931088596884);
#1088=CONICAL_SURFACE('',#19236,1.61,0.959931088596878);
#1089=CONICAL_SURFACE('',#19241,2.,0.959931088596884);
#1090=CONICAL_SURFACE('',#19245,1.61,0.959931088596878);
#1091=CONICAL_SURFACE('',#19250,2.,0.959931088596884);
#1092=CONICAL_SURFACE('',#19254,1.61,0.959931088596878);
#1093=CONICAL_SURFACE('',#19259,2.,0.959931088596884);
#1094=CONICAL_SURFACE('',#19263,1.61,0.959931088596878);
#1095=CONICAL_SURFACE('',#19268,2.,0.959931088596884);
#1096=CONICAL_SURFACE('',#19272,1.61,0.959931088596878);
#1097=CONICAL_SURFACE('',#19277,2.,0.959931088596884);
#1098=CONICAL_SURFACE('',#19281,1.61,0.959931088596878);
#1099=CONICAL_SURFACE('',#19286,2.,0.959931088596884);
#1100=CONICAL_SURFACE('',#19290,1.61,0.959931088596878);
#1101=CONICAL_SURFACE('',#19295,2.,0.959931088596884);
#1102=CONICAL_SURFACE('',#19299,1.61,0.959931088596878);
#1103=CONICAL_SURFACE('',#19304,2.,0.959931088596884);
#1104=CONICAL_SURFACE('',#19308,1.61,0.959931088596878);
#1105=CONICAL_SURFACE('',#19313,2.,0.959931088596884);
#1106=CONICAL_SURFACE('',#19317,1.61,0.959931088596878);
#1107=CONICAL_SURFACE('',#19322,2.,0.959931088596884);
#1108=CONICAL_SURFACE('',#19326,1.61,0.959931088596878);
#1109=CONICAL_SURFACE('',#19331,2.,0.959931088596884);
#1110=CONICAL_SURFACE('',#19334,8.175,0.785398163397449);
#1111=CONICAL_SURFACE('',#19413,8.175,0.785398163397449);
#1112=SHAPE_REPRESENTATION_RELATIONSHIP('SRR','None',#38685,#1126);
#1113=SHAPE_REPRESENTATION_RELATIONSHIP('SRR','None',#38686,#1127);
#1114=SHAPE_REPRESENTATION_RELATIONSHIP('SRR','None',#38687,#1128);
#1115=SHAPE_REPRESENTATION_RELATIONSHIP('SRR','None',#38688,#1129);
#1116=SHAPE_REPRESENTATION_RELATIONSHIP('SRR','None',#38689,#1130);
#1117=SHAPE_REPRESENTATION_RELATIONSHIP('SRR','None',#38690,#1131);
#1118=SHAPE_REPRESENTATION_RELATIONSHIP('SRR','None',#38691,#1132);
#1119=SHAPE_REPRESENTATION_RELATIONSHIP('SRR','None',#38692,#1133);
#1120=SHAPE_REPRESENTATION_RELATIONSHIP('SRR','None',#38693,#1134);
#1121=SHAPE_REPRESENTATION_RELATIONSHIP('SRR','None',#38694,#1135);
#1122=SHAPE_REPRESENTATION_RELATIONSHIP('SRR','None',#38695,#1136);
#1123=SHAPE_REPRESENTATION_RELATIONSHIP('SRR','None',#38696,#1137);
#1124=SHAPE_REPRESENTATION_RELATIONSHIP('SRR','None',#38697,#1138);
#1125=SHAPE_REPRESENTATION_RELATIONSHIP('SRR','None',#38698,#1139);
#1126=ADVANCED_BREP_SHAPE_REPRESENTATION('',(#1166,#1167,#1168,#1169),#38621);
#1127=ADVANCED_BREP_SHAPE_REPRESENTATION('',(#1170,#1171,#1172,#1173),#38622);
#1128=ADVANCED_BREP_SHAPE_REPRESENTATION('',(#1174),#38623);
#1129=ADVANCED_BREP_SHAPE_REPRESENTATION('',(#1175),#38624);
#1130=ADVANCED_BREP_SHAPE_REPRESENTATION('',(#1176),#38625);
#1131=ADVANCED_BREP_SHAPE_REPRESENTATION('',(#1177),#38626);
#1132=ADVANCED_BREP_SHAPE_REPRESENTATION('',(#1178),#38627);
#1133=ADVANCED_BREP_SHAPE_REPRESENTATION('',(#1179),#38628);
#1134=ADVANCED_BREP_SHAPE_REPRESENTATION('',(#1180),#38629);
#1135=ADVANCED_BREP_SHAPE_REPRESENTATION('',(#1181),#38630);
#1136=ADVANCED_BREP_SHAPE_REPRESENTATION('',(#1182),#38631);
#1137=ADVANCED_BREP_SHAPE_REPRESENTATION('',(#1183),#38632);
#1138=ADVANCED_BREP_SHAPE_REPRESENTATION('',(#1184),#38633);
#1139=ADVANCED_BREP_SHAPE_REPRESENTATION('',(#1185,#1186,#1187,#1188,#1189,
#1190,#1191),#38634);
#1140=STYLED_ITEM('',(#38764),#1166);
#1141=STYLED_ITEM('',(#38764),#1167);
#1142=STYLED_ITEM('',(#38764),#1168);
#1143=STYLED_ITEM('',(#38764),#1169);
#1144=STYLED_ITEM('',(#38765),#1170);
#1145=STYLED_ITEM('',(#38765),#1171);
#1146=STYLED_ITEM('',(#38765),#1172);
#1147=STYLED_ITEM('',(#38765),#1173);
#1148=STYLED_ITEM('',(#38766),#1174);
#1149=STYLED_ITEM('',(#38766),#1175);
#1150=STYLED_ITEM('',(#38766),#1176);
#1151=STYLED_ITEM('',(#38767),#1177);
#1152=STYLED_ITEM('',(#38768),#1178);
#1153=STYLED_ITEM('',(#38767),#1179);
#1154=STYLED_ITEM('',(#38765),#1180);
#1155=STYLED_ITEM('',(#38767),#1181);
#1156=STYLED_ITEM('',(#38765),#1182);
#1157=STYLED_ITEM('',(#38769),#1183);
#1158=STYLED_ITEM('',(#38765),#1184);
#1159=STYLED_ITEM('',(#38765),#1185);
#1160=STYLED_ITEM('',(#38765),#1186);
#1161=STYLED_ITEM('',(#38765),#1187);
#1162=STYLED_ITEM('',(#38765),#1188);
#1163=STYLED_ITEM('',(#38765),#1189);
#1164=STYLED_ITEM('',(#38765),#1190);
#1165=STYLED_ITEM('',(#38765),#1191);
#1166=MANIFOLD_SOLID_BREP('Body1',#17606);
#1167=MANIFOLD_SOLID_BREP('Body2',#17607);
#1168=MANIFOLD_SOLID_BREP('Body3',#17608);
#1169=MANIFOLD_SOLID_BREP('Body4',#17609);
#1170=MANIFOLD_SOLID_BREP('Body1',#17610);
#1171=MANIFOLD_SOLID_BREP('Body2',#17611);
#1172=MANIFOLD_SOLID_BREP('Body3',#17612);
#1173=MANIFOLD_SOLID_BREP('Body4',#17613);
#1174=MANIFOLD_SOLID_BREP('Body1',#17614);
#1175=MANIFOLD_SOLID_BREP('Body1',#17615);
#1176=MANIFOLD_SOLID_BREP('Body1',#17616);
#1177=MANIFOLD_SOLID_BREP('Body1',#17617);
#1178=MANIFOLD_SOLID_BREP('Body1',#17618);
#1179=MANIFOLD_SOLID_BREP('Body1',#17619);
#1180=MANIFOLD_SOLID_BREP('Body1',#17620);
#1181=MANIFOLD_SOLID_BREP('Body1',#17621);
#1182=MANIFOLD_SOLID_BREP('Body1',#17622);
#1183=MANIFOLD_SOLID_BREP('Body1',#17623);
#1184=MANIFOLD_SOLID_BREP('Body1',#17624);
#1185=MANIFOLD_SOLID_BREP('Body1',#17625);
#1186=MANIFOLD_SOLID_BREP('Body2',#17626);
#1187=MANIFOLD_SOLID_BREP('Body3',#17627);
#1188=MANIFOLD_SOLID_BREP('Body4',#17628);
#1189=MANIFOLD_SOLID_BREP('Body5',#17629);
#1190=MANIFOLD_SOLID_BREP('Body6',#17630);
#1191=MANIFOLD_SOLID_BREP('Body7',#17631);
#1192=PLANE('',#17795);
#1193=PLANE('',#17796);
#1194=PLANE('',#17797);
#1195=PLANE('',#17800);
#1196=PLANE('',#17803);
#1197=PLANE('',#17804);
#1198=PLANE('',#17816);
#1199=PLANE('',#17817);
#1200=PLANE('',#17818);
#1201=PLANE('',#17819);
#1202=PLANE('',#17821);
#1203=PLANE('',#17824);
#1204=PLANE('',#17825);
#1205=PLANE('',#17826);
#1206=PLANE('',#17827);
#1207=PLANE('',#17828);
#1208=PLANE('',#17831);
#1209=PLANE('',#17835);
#1210=PLANE('',#17838);
#1211=PLANE('',#17841);
#1212=PLANE('',#17842);
#1213=PLANE('',#17843);
#1214=PLANE('',#17844);
#1215=PLANE('',#17847);
#1216=PLANE('',#17851);
#1217=PLANE('',#17854);
#1218=PLANE('',#17861);
#1219=PLANE('',#17863);
#1220=PLANE('',#17864);
#1221=PLANE('',#17865);
#1222=PLANE('',#17874);
#1223=PLANE('',#17875);
#1224=PLANE('',#17876);
#1225=PLANE('',#17877);
#1226=PLANE('',#17878);
#1227=PLANE('',#17879);
#1228=PLANE('',#17880);
#1229=PLANE('',#17881);
#1230=PLANE('',#17882);
#1231=PLANE('',#17885);
#1232=PLANE('',#17888);
#1233=PLANE('',#17889);
#1234=PLANE('',#17906);
#1235=PLANE('',#17907);
#1236=PLANE('',#17908);
#1237=PLANE('',#17993);
#1238=PLANE('',#17994);
#1239=PLANE('',#17995);
#1240=PLANE('',#17996);
#1241=PLANE('',#17997);
#1242=PLANE('',#17998);
#1243=PLANE('',#17999);
#1244=PLANE('',#18000);
#1245=PLANE('',#18009);
#1246=PLANE('',#18010);
#1247=PLANE('',#18011);
#1248=PLANE('',#18019);
#1249=PLANE('',#18020);
#1250=PLANE('',#18034);
#1251=PLANE('',#18035);
#1252=PLANE('',#18055);
#1253=PLANE('',#18056);
#1254=PLANE('',#18057);
#1255=PLANE('',#18088);
#1256=PLANE('',#18089);
#1257=PLANE('',#18091);
#1258=PLANE('',#18100);
#1259=PLANE('',#18102);
#1260=PLANE('',#18146);
#1261=PLANE('',#18147);
#1262=PLANE('',#18148);
#1263=PLANE('',#18182);
#1264=PLANE('',#18183);
#1265=PLANE('',#18185);
#1266=PLANE('',#18187);
#1267=PLANE('',#18189);
#1268=PLANE('',#18215);
#1269=PLANE('',#18216);
#1270=PLANE('',#18217);
#1271=PLANE('',#18240);
#1272=PLANE('',#18241);
#1273=PLANE('',#18242);
#1274=PLANE('',#18243);
#1275=PLANE('',#18356);
#1276=PLANE('',#18362);
#1277=PLANE('',#18367);
#1278=PLANE('',#18368);
#1279=PLANE('',#18491);
#1280=PLANE('',#18492);
#1281=PLANE('',#18493);
#1282=PLANE('',#18496);
#1283=PLANE('',#18497);
#1284=PLANE('',#18500);
#1285=PLANE('',#18501);
#1286=PLANE('',#18502);
#1287=PLANE('',#18504);
#1288=PLANE('',#18509);
#1289=PLANE('',#18510);
#1290=PLANE('',#18514);
#1291=PLANE('',#18515);
#1292=PLANE('',#18516);
#1293=PLANE('',#18517);
#1294=PLANE('',#18518);
#1295=PLANE('',#18519);
#1296=PLANE('',#18520);
#1297=PLANE('',#18522);
#1298=PLANE('',#18523);
#1299=PLANE('',#18524);
#1300=PLANE('',#18527);
#1301=PLANE('',#18529);
#1302=PLANE('',#18608);
#1303=PLANE('',#18609);
#1304=PLANE('',#18630);
#1305=PLANE('',#18634);
#1306=PLANE('',#18635);
#1307=PLANE('',#18636);
#1308=PLANE('',#18638);
#1309=PLANE('',#18639);
#1310=PLANE('',#18642);
#1311=PLANE('',#18643);
#1312=PLANE('',#18644);
#1313=PLANE('',#18645);
#1314=PLANE('',#18646);
#1315=PLANE('',#18647);
#1316=PLANE('',#18648);
#1317=PLANE('',#18649);
#1318=PLANE('',#18655);
#1319=PLANE('',#19031);
#1320=PLANE('',#19033);
#1321=PLANE('',#19034);
#1322=PLANE('',#19035);
#1323=PLANE('',#19036);
#1324=PLANE('',#19037);
#1325=PLANE('',#19038);
#1326=PLANE('',#19039);
#1327=PLANE('',#19040);
#1328=PLANE('',#19041);
#1329=PLANE('',#19042);
#1330=PLANE('',#19043);
#1331=PLANE('',#19044);
#1332=PLANE('',#19045);
#1333=PLANE('',#19046);
#1334=PLANE('',#19047);
#1335=PLANE('',#19048);
#1336=PLANE('',#19049);
#1337=PLANE('',#19050);
#1338=PLANE('',#19051);
#1339=PLANE('',#19052);
#1340=PLANE('',#19053);
#1341=PLANE('',#19054);
#1342=PLANE('',#19055);
#1343=PLANE('',#19056);
#1344=PLANE('',#19057);
#1345=PLANE('',#19058);
#1346=PLANE('',#19059);
#1347=PLANE('',#19060);
#1348=PLANE('',#19061);
#1349=PLANE('',#19062);
#1350=PLANE('',#19063);
#1351=PLANE('',#19064);
#1352=PLANE('',#19065);
#1353=PLANE('',#19066);
#1354=PLANE('',#19067);
#1355=PLANE('',#19068);
#1356=PLANE('',#19069);
#1357=PLANE('',#19070);
#1358=PLANE('',#19071);
#1359=PLANE('',#19072);
#1360=PLANE('',#19073);
#1361=PLANE('',#19074);
#1362=PLANE('',#19075);
#1363=PLANE('',#19076);
#1364=PLANE('',#19077);
#1365=PLANE('',#19078);
#1366=PLANE('',#19079);
#1367=PLANE('',#19080);
#1368=PLANE('',#19081);
#1369=PLANE('',#19082);
#1370=PLANE('',#19083);
#1371=PLANE('',#19084);
#1372=PLANE('',#19085);
#1373=PLANE('',#19086);
#1374=PLANE('',#19087);
#1375=PLANE('',#19088);
#1376=PLANE('',#19089);
#1377=PLANE('',#19090);
#1378=PLANE('',#19091);
#1379=PLANE('',#19092);
#1380=PLANE('',#19093);
#1381=PLANE('',#19094);
#1382=PLANE('',#19095);
#1383=PLANE('',#19096);
#1384=PLANE('',#19097);
#1385=PLANE('',#19098);
#1386=PLANE('',#19099);
#1387=PLANE('',#19100);
#1388=PLANE('',#19101);
#1389=PLANE('',#19102);
#1390=PLANE('',#19103);
#1391=PLANE('',#19104);
#1392=PLANE('',#19105);
#1393=PLANE('',#19106);
#1394=PLANE('',#19107);
#1395=PLANE('',#19108);
#1396=PLANE('',#19109);
#1397=PLANE('',#19110);
#1398=PLANE('',#19111);
#1399=PLANE('',#19112);
#1400=PLANE('',#19113);
#1401=PLANE('',#19114);
#1402=PLANE('',#19115);
#1403=PLANE('',#19116);
#1404=PLANE('',#19117);
#1405=PLANE('',#19118);
#1406=PLANE('',#19119);
#1407=PLANE('',#19120);
#1408=PLANE('',#19121);
#1409=PLANE('',#19122);
#1410=PLANE('',#19123);
#1411=PLANE('',#19124);
#1412=PLANE('',#19125);
#1413=PLANE('',#19126);
#1414=PLANE('',#19127);
#1415=PLANE('',#19128);
#1416=PLANE('',#19129);
#1417=PLANE('',#19130);
#1418=PLANE('',#19131);
#1419=PLANE('',#19132);
#1420=PLANE('',#19133);
#1421=PLANE('',#19134);
#1422=PLANE('',#19135);
#1423=PLANE('',#19136);
#1424=PLANE('',#19137);
#1425=PLANE('',#19138);
#1426=PLANE('',#19139);
#1427=PLANE('',#19140);
#1428=PLANE('',#19141);
#1429=PLANE('',#19142);
#1430=PLANE('',#19143);
#1431=PLANE('',#19144);
#1432=PLANE('',#19145);
#1433=PLANE('',#19146);
#1434=PLANE('',#19147);
#1435=PLANE('',#19148);
#1436=PLANE('',#19149);
#1437=PLANE('',#19150);
#1438=PLANE('',#19151);
#1439=PLANE('',#19152);
#1440=PLANE('',#19153);
#1441=PLANE('',#19154);
#1442=PLANE('',#19155);
#1443=PLANE('',#19156);
#1444=PLANE('',#19157);
#1445=PLANE('',#19158);
#1446=PLANE('',#19159);
#1447=PLANE('',#19160);
#1448=PLANE('',#19161);
#1449=PLANE('',#19162);
#1450=PLANE('',#19163);
#1451=PLANE('',#19164);
#1452=PLANE('',#19165);
#1453=PLANE('',#19166);
#1454=PLANE('',#19167);
#1455=PLANE('',#19168);
#1456=PLANE('',#19169);
#1457=PLANE('',#19170);
#1458=PLANE('',#19171);
#1459=PLANE('',#19172);
#1460=PLANE('',#19173);
#1461=PLANE('',#19174);
#1462=PLANE('',#19175);
#1463=PLANE('',#19176);
#1464=PLANE('',#19177);
#1465=PLANE('',#19178);
#1466=PLANE('',#19179);
#1467=PLANE('',#19180);
#1468=PLANE('',#19181);
#1469=PLANE('',#19182);
#1470=PLANE('',#19183);
#1471=PLANE('',#19184);
#1472=PLANE('',#19185);
#1473=PLANE('',#19186);
#1474=PLANE('',#19187);
#1475=PLANE('',#19188);
#1476=PLANE('',#19203);
#1477=PLANE('',#19204);
#1478=PLANE('',#19205);
#1479=PLANE('',#19206);
#1480=PLANE('',#19207);
#1481=PLANE('',#19208);
#1482=PLANE('',#19209);
#1483=PLANE('',#19570);
#1484=PLANE('',#19572);
#1485=PLANE('',#19573);
#1486=PLANE('',#19574);
#1487=PLANE('',#19575);
#1488=PLANE('',#19576);
#1489=PLANE('',#19577);
#1490=PLANE('',#19578);
#1491=PLANE('',#19579);
#1492=PLANE('',#19580);
#1493=PLANE('',#19581);
#1494=PLANE('',#19582);
#1495=PLANE('',#19583);
#1496=PLANE('',#19584);
#1497=PLANE('',#19585);
#1498=PLANE('',#19586);
#1499=PLANE('',#19587);
#1500=PLANE('',#19588);
#1501=PLANE('',#19589);
#1502=PLANE('',#19590);
#1503=PLANE('',#19591);
#1504=PLANE('',#19592);
#1505=PLANE('',#19593);
#1506=PLANE('',#19594);
#1507=PLANE('',#19595);
#1508=PLANE('',#19596);
#1509=PLANE('',#19597);
#1510=PLANE('',#19598);
#1511=PLANE('',#19599);
#1512=PLANE('',#19600);
#1513=PLANE('',#19601);
#1514=PLANE('',#19602);
#1515=PLANE('',#19603);
#1516=PLANE('',#19604);
#1517=PLANE('',#19605);
#1518=PLANE('',#19606);
#1519=PLANE('',#19607);
#1520=PLANE('',#19608);
#1521=PLANE('',#19609);
#1522=PLANE('',#19610);
#1523=PLANE('',#19611);
#1524=PLANE('',#19612);
#1525=PLANE('',#19613);
#1526=PLANE('',#19614);
#1527=PLANE('',#19615);
#1528=PLANE('',#19616);
#1529=PLANE('',#19617);
#1530=PLANE('',#19618);
#1531=PLANE('',#19619);
#1532=PLANE('',#19620);
#1533=PLANE('',#19621);
#1534=PLANE('',#19622);
#1535=PLANE('',#19623);
#1536=PLANE('',#19624);
#1537=PLANE('',#19625);
#1538=PLANE('',#19626);
#1539=PLANE('',#19627);
#1540=PLANE('',#19628);
#1541=PLANE('',#19629);
#1542=PLANE('',#19630);
#1543=PLANE('',#19631);
#1544=PLANE('',#19632);
#1545=PLANE('',#19633);
#1546=PLANE('',#19634);
#1547=PLANE('',#19635);
#1548=PLANE('',#19636);
#1549=PLANE('',#19637);
#1550=PLANE('',#19638);
#1551=PLANE('',#19639);
#1552=PLANE('',#19640);
#1553=PLANE('',#19641);
#1554=PLANE('',#19642);
#1555=PLANE('',#19643);
#1556=PLANE('',#19644);
#1557=PLANE('',#19645);
#1558=PLANE('',#19646);
#1559=PLANE('',#19647);
#1560=PLANE('',#19648);
#1561=PLANE('',#19649);
#1562=PLANE('',#19650);
#1563=PLANE('',#19651);
#1564=PLANE('',#19652);
#1565=PLANE('',#19653);
#1566=PLANE('',#19654);
#1567=PLANE('',#19655);
#1568=PLANE('',#19656);
#1569=PLANE('',#19657);
#1570=PLANE('',#19658);
#1571=PLANE('',#19659);
#1572=PLANE('',#19660);
#1573=PLANE('',#19661);
#1574=PLANE('',#19662);
#1575=PLANE('',#19663);
#1576=PLANE('',#19664);
#1577=PLANE('',#19665);
#1578=PLANE('',#19666);
#1579=PLANE('',#19667);
#1580=PLANE('',#19668);
#1581=PLANE('',#19669);
#1582=PLANE('',#19670);
#1583=PLANE('',#19671);
#1584=PLANE('',#19672);
#1585=PLANE('',#19673);
#1586=PLANE('',#19674);
#1587=PLANE('',#19675);
#1588=PLANE('',#19676);
#1589=PLANE('',#19677);
#1590=PLANE('',#19678);
#1591=PLANE('',#19679);
#1592=PLANE('',#19680);
#1593=PLANE('',#19681);
#1594=PLANE('',#19682);
#1595=PLANE('',#19683);
#1596=PLANE('',#19684);
#1597=PLANE('',#19685);
#1598=PLANE('',#19686);
#1599=PLANE('',#19687);
#1600=PLANE('',#19688);
#1601=PLANE('',#19689);
#1602=PLANE('',#19690);
#1603=PLANE('',#19691);
#1604=PLANE('',#19692);
#1605=PLANE('',#19693);
#1606=PLANE('',#19694);
#1607=PLANE('',#19695);
#1608=PLANE('',#19696);
#1609=PLANE('',#19697);
#1610=PLANE('',#19698);
#1611=PLANE('',#19699);
#1612=PLANE('',#19700);
#1613=PLANE('',#19701);
#1614=PLANE('',#19702);
#1615=PLANE('',#19703);
#1616=PLANE('',#19704);
#1617=PLANE('',#19705);
#1618=PLANE('',#19706);
#1619=PLANE('',#19707);
#1620=PLANE('',#19708);
#1621=PLANE('',#19709);
#1622=PLANE('',#19710);
#1623=PLANE('',#19711);
#1624=PLANE('',#19712);
#1625=PLANE('',#19713);
#1626=PLANE('',#19714);
#1627=PLANE('',#19715);
#1628=PLANE('',#19716);
#1629=PLANE('',#19717);
#1630=PLANE('',#19718);
#1631=PLANE('',#19719);
#1632=PLANE('',#19720);
#1633=PLANE('',#19721);
#1634=PLANE('',#19722);
#1635=PLANE('',#19723);
#1636=PLANE('',#19724);
#1637=PLANE('',#19725);
#1638=PLANE('',#19726);
#1639=PLANE('',#19727);
#1640=PLANE('',#19728);
#1641=FACE_OUTER_BOUND('',#2647,.T.);
#1642=FACE_OUTER_BOUND('',#2648,.T.);
#1643=FACE_OUTER_BOUND('',#2649,.T.);
#1644=FACE_OUTER_BOUND('',#2650,.T.);
#1645=FACE_OUTER_BOUND('',#2651,.T.);
#1646=FACE_OUTER_BOUND('',#2652,.T.);
#1647=FACE_OUTER_BOUND('',#2653,.T.);
#1648=FACE_OUTER_BOUND('',#2654,.T.);
#1649=FACE_OUTER_BOUND('',#2655,.T.);
#1650=FACE_OUTER_BOUND('',#2656,.T.);
#1651=FACE_OUTER_BOUND('',#2657,.T.);
#1652=FACE_OUTER_BOUND('',#2658,.T.);
#1653=FACE_OUTER_BOUND('',#2659,.T.);
#1654=FACE_OUTER_BOUND('',#2660,.T.);
#1655=FACE_OUTER_BOUND('',#2661,.T.);
#1656=FACE_OUTER_BOUND('',#2662,.T.);
#1657=FACE_OUTER_BOUND('',#2663,.T.);
#1658=FACE_OUTER_BOUND('',#2664,.T.);
#1659=FACE_OUTER_BOUND('',#2665,.T.);
#1660=FACE_OUTER_BOUND('',#2666,.T.);
#1661=FACE_OUTER_BOUND('',#2667,.T.);
#1662=FACE_OUTER_BOUND('',#2668,.T.);
#1663=FACE_OUTER_BOUND('',#2669,.T.);
#1664=FACE_OUTER_BOUND('',#2670,.T.);
#1665=FACE_OUTER_BOUND('',#2671,.T.);
#1666=FACE_OUTER_BOUND('',#2672,.T.);
#1667=FACE_OUTER_BOUND('',#2673,.T.);
#1668=FACE_OUTER_BOUND('',#2674,.T.);
#1669=FACE_OUTER_BOUND('',#2675,.T.);
#1670=FACE_OUTER_BOUND('',#2676,.T.);
#1671=FACE_OUTER_BOUND('',#2677,.T.);
#1672=FACE_OUTER_BOUND('',#2678,.T.);
#1673=FACE_OUTER_BOUND('',#2679,.T.);
#1674=FACE_OUTER_BOUND('',#2680,.T.);
#1675=FACE_OUTER_BOUND('',#2681,.T.);
#1676=FACE_OUTER_BOUND('',#2682,.T.);
#1677=FACE_OUTER_BOUND('',#2683,.T.);
#1678=FACE_OUTER_BOUND('',#2684,.T.);
#1679=FACE_OUTER_BOUND('',#2685,.T.);
#1680=FACE_OUTER_BOUND('',#2686,.T.);
#1681=FACE_OUTER_BOUND('',#2687,.T.);
#1682=FACE_OUTER_BOUND('',#2688,.T.);
#1683=FACE_OUTER_BOUND('',#2689,.T.);
#1684=FACE_OUTER_BOUND('',#2690,.T.);
#1685=FACE_OUTER_BOUND('',#2691,.T.);
#1686=FACE_OUTER_BOUND('',#2692,.T.);
#1687=FACE_OUTER_BOUND('',#2693,.T.);
#1688=FACE_OUTER_BOUND('',#2694,.T.);
#1689=FACE_OUTER_BOUND('',#2695,.T.);
#1690=FACE_OUTER_BOUND('',#2696,.T.);
#1691=FACE_OUTER_BOUND('',#2697,.T.);
#1692=FACE_OUTER_BOUND('',#2698,.T.);
#1693=FACE_OUTER_BOUND('',#2699,.T.);
#1694=FACE_OUTER_BOUND('',#2700,.T.);
#1695=FACE_OUTER_BOUND('',#2701,.T.);
#1696=FACE_OUTER_BOUND('',#2702,.T.);
#1697=FACE_OUTER_BOUND('',#2703,.T.);
#1698=FACE_OUTER_BOUND('',#2704,.T.);
#1699=FACE_OUTER_BOUND('',#2705,.T.);
#1700=FACE_OUTER_BOUND('',#2706,.T.);
#1701=FACE_OUTER_BOUND('',#2707,.T.);
#1702=FACE_OUTER_BOUND('',#2708,.T.);
#1703=FACE_OUTER_BOUND('',#2709,.T.);
#1704=FACE_OUTER_BOUND('',#2710,.T.);
#1705=FACE_OUTER_BOUND('',#2711,.T.);
#1706=FACE_OUTER_BOUND('',#2712,.T.);
#1707=FACE_OUTER_BOUND('',#2713,.T.);
#1708=FACE_OUTER_BOUND('',#2715,.T.);
#1709=FACE_OUTER_BOUND('',#2716,.T.);
#1710=FACE_OUTER_BOUND('',#2718,.T.);
#1711=FACE_OUTER_BOUND('',#2719,.T.);
#1712=FACE_OUTER_BOUND('',#2720,.T.);
#1713=FACE_OUTER_BOUND('',#2721,.T.);
#1714=FACE_OUTER_BOUND('',#2722,.T.);
#1715=FACE_OUTER_BOUND('',#2723,.T.);
#1716=FACE_OUTER_BOUND('',#2724,.T.);
#1717=FACE_OUTER_BOUND('',#2725,.T.);
#1718=FACE_OUTER_BOUND('',#2726,.T.);
#1719=FACE_OUTER_BOUND('',#2727,.T.);
#1720=FACE_OUTER_BOUND('',#2728,.T.);
#1721=FACE_OUTER_BOUND('',#2729,.T.);
#1722=FACE_OUTER_BOUND('',#2730,.T.);
#1723=FACE_OUTER_BOUND('',#2731,.T.);
#1724=FACE_OUTER_BOUND('',#2732,.T.);
#1725=FACE_OUTER_BOUND('',#2733,.T.);
#1726=FACE_OUTER_BOUND('',#2734,.T.);
#1727=FACE_OUTER_BOUND('',#2735,.T.);
#1728=FACE_OUTER_BOUND('',#2736,.T.);
#1729=FACE_OUTER_BOUND('',#2737,.T.);
#1730=FACE_OUTER_BOUND('',#2738,.T.);
#1731=FACE_OUTER_BOUND('',#2739,.T.);
#1732=FACE_OUTER_BOUND('',#2740,.T.);
#1733=FACE_OUTER_BOUND('',#2741,.T.);
#1734=FACE_OUTER_BOUND('',#2742,.T.);
#1735=FACE_OUTER_BOUND('',#2743,.T.);
#1736=FACE_OUTER_BOUND('',#2744,.T.);
#1737=FACE_OUTER_BOUND('',#2745,.T.);
#1738=FACE_OUTER_BOUND('',#2746,.T.);
#1739=FACE_OUTER_BOUND('',#2747,.T.);
#1740=FACE_OUTER_BOUND('',#2748,.T.);
#1741=FACE_OUTER_BOUND('',#2749,.T.);
#1742=FACE_OUTER_BOUND('',#2750,.T.);
#1743=FACE_OUTER_BOUND('',#2751,.T.);
#1744=FACE_OUTER_BOUND('',#2752,.T.);
#1745=FACE_OUTER_BOUND('',#2753,.T.);
#1746=FACE_OUTER_BOUND('',#2754,.T.);
#1747=FACE_OUTER_BOUND('',#2755,.T.);
#1748=FACE_OUTER_BOUND('',#2756,.T.);
#1749=FACE_OUTER_BOUND('',#2757,.T.);
#1750=FACE_OUTER_BOUND('',#2758,.T.);
#1751=FACE_OUTER_BOUND('',#2759,.T.);
#1752=FACE_OUTER_BOUND('',#2760,.T.);
#1753=FACE_OUTER_BOUND('',#2761,.T.);
#1754=FACE_OUTER_BOUND('',#2762,.T.);
#1755=FACE_OUTER_BOUND('',#2763,.T.);
#1756=FACE_OUTER_BOUND('',#2764,.T.);
#1757=FACE_OUTER_BOUND('',#2765,.T.);
#1758=FACE_OUTER_BOUND('',#2766,.T.);
#1759=FACE_OUTER_BOUND('',#2767,.T.);
#1760=FACE_OUTER_BOUND('',#2768,.T.);
#1761=FACE_OUTER_BOUND('',#2769,.T.);
#1762=FACE_OUTER_BOUND('',#2770,.T.);
#1763=FACE_OUTER_BOUND('',#2771,.T.);
#1764=FACE_OUTER_BOUND('',#2772,.T.);
#1765=FACE_OUTER_BOUND('',#2773,.T.);
#1766=FACE_OUTER_BOUND('',#2774,.T.);
#1767=FACE_OUTER_BOUND('',#2775,.T.);
#1768=FACE_OUTER_BOUND('',#2776,.T.);
#1769=FACE_OUTER_BOUND('',#2777,.T.);
#1770=FACE_OUTER_BOUND('',#2778,.T.);
#1771=FACE_OUTER_BOUND('',#2780,.T.);
#1772=FACE_OUTER_BOUND('',#2782,.T.);
#1773=FACE_OUTER_BOUND('',#2784,.T.);
#1774=FACE_OUTER_BOUND('',#2786,.T.);
#1775=FACE_OUTER_BOUND('',#2788,.T.);
#1776=FACE_OUTER_BOUND('',#2789,.T.);
#1777=FACE_OUTER_BOUND('',#2790,.T.);
#1778=FACE_OUTER_BOUND('',#2791,.T.);
#1779=FACE_OUTER_BOUND('',#2792,.T.);
#1780=FACE_OUTER_BOUND('',#2793,.T.);
#1781=FACE_OUTER_BOUND('',#2794,.T.);
#1782=FACE_OUTER_BOUND('',#2795,.T.);
#1783=FACE_OUTER_BOUND('',#2796,.T.);
#1784=FACE_OUTER_BOUND('',#2797,.T.);
#1785=FACE_OUTER_BOUND('',#2798,.T.);
#1786=FACE_OUTER_BOUND('',#2799,.T.);
#1787=FACE_OUTER_BOUND('',#2801,.T.);
#1788=FACE_OUTER_BOUND('',#2802,.T.);
#1789=FACE_OUTER_BOUND('',#2803,.T.);
#1790=FACE_OUTER_BOUND('',#2804,.T.);
#1791=FACE_OUTER_BOUND('',#2806,.T.);
#1792=FACE_OUTER_BOUND('',#2808,.T.);
#1793=FACE_OUTER_BOUND('',#2809,.T.);
#1794=FACE_OUTER_BOUND('',#2810,.T.);
#1795=FACE_OUTER_BOUND('',#2811,.T.);
#1796=FACE_OUTER_BOUND('',#2812,.T.);
#1797=FACE_OUTER_BOUND('',#2813,.T.);
#1798=FACE_OUTER_BOUND('',#2814,.T.);
#1799=FACE_OUTER_BOUND('',#2815,.T.);
#1800=FACE_OUTER_BOUND('',#2816,.T.);
#1801=FACE_OUTER_BOUND('',#2817,.T.);
#1802=FACE_OUTER_BOUND('',#2818,.T.);
#1803=FACE_OUTER_BOUND('',#2819,.T.);
#1804=FACE_OUTER_BOUND('',#2821,.T.);
#1805=FACE_OUTER_BOUND('',#2822,.T.);
#1806=FACE_OUTER_BOUND('',#2824,.T.);
#1807=FACE_OUTER_BOUND('',#2825,.T.);
#1808=FACE_OUTER_BOUND('',#2827,.T.);
#1809=FACE_OUTER_BOUND('',#2828,.T.);
#1810=FACE_OUTER_BOUND('',#2829,.T.);
#1811=FACE_OUTER_BOUND('',#2830,.T.);
#1812=FACE_OUTER_BOUND('',#2831,.T.);
#1813=FACE_OUTER_BOUND('',#2832,.T.);
#1814=FACE_OUTER_BOUND('',#2833,.T.);
#1815=FACE_OUTER_BOUND('',#2834,.T.);
#1816=FACE_OUTER_BOUND('',#2835,.T.);
#1817=FACE_OUTER_BOUND('',#2836,.T.);
#1818=FACE_OUTER_BOUND('',#2838,.T.);
#1819=FACE_OUTER_BOUND('',#2839,.T.);
#1820=FACE_OUTER_BOUND('',#2840,.T.);
#1821=FACE_OUTER_BOUND('',#2841,.T.);
#1822=FACE_OUTER_BOUND('',#2842,.T.);
#1823=FACE_OUTER_BOUND('',#2843,.T.);
#1824=FACE_OUTER_BOUND('',#2844,.T.);
#1825=FACE_OUTER_BOUND('',#2845,.T.);
#1826=FACE_OUTER_BOUND('',#2846,.T.);
#1827=FACE_OUTER_BOUND('',#2847,.T.);
#1828=FACE_OUTER_BOUND('',#2848,.T.);
#1829=FACE_OUTER_BOUND('',#2849,.T.);
#1830=FACE_OUTER_BOUND('',#2850,.T.);
#1831=FACE_OUTER_BOUND('',#2851,.T.);
#1832=FACE_OUTER_BOUND('',#2852,.T.);
#1833=FACE_OUTER_BOUND('',#2853,.T.);
#1834=FACE_OUTER_BOUND('',#2854,.T.);
#1835=FACE_OUTER_BOUND('',#2855,.T.);
#1836=FACE_OUTER_BOUND('',#2856,.T.);
#1837=FACE_OUTER_BOUND('',#2857,.T.);
#1838=FACE_OUTER_BOUND('',#2858,.T.);
#1839=FACE_OUTER_BOUND('',#2859,.T.);
#1840=FACE_OUTER_BOUND('',#2860,.T.);
#1841=FACE_OUTER_BOUND('',#2861,.T.);
#1842=FACE_OUTER_BOUND('',#2862,.T.);
#1843=FACE_OUTER_BOUND('',#2863,.T.);
#1844=FACE_OUTER_BOUND('',#2864,.T.);
#1845=FACE_OUTER_BOUND('',#2865,.T.);
#1846=FACE_OUTER_BOUND('',#2866,.T.);
#1847=FACE_OUTER_BOUND('',#2867,.T.);
#1848=FACE_OUTER_BOUND('',#2868,.T.);
#1849=FACE_OUTER_BOUND('',#2869,.T.);
#1850=FACE_OUTER_BOUND('',#2870,.T.);
#1851=FACE_OUTER_BOUND('',#2872,.T.);
#1852=FACE_OUTER_BOUND('',#2874,.T.);
#1853=FACE_OUTER_BOUND('',#2875,.T.);
#1854=FACE_OUTER_BOUND('',#2876,.T.);
#1855=FACE_OUTER_BOUND('',#2877,.T.);
#1856=FACE_OUTER_BOUND('',#2878,.T.);
#1857=FACE_OUTER_BOUND('',#2879,.T.);
#1858=FACE_OUTER_BOUND('',#2880,.T.);
#1859=FACE_OUTER_BOUND('',#2881,.T.);
#1860=FACE_OUTER_BOUND('',#2882,.T.);
#1861=FACE_OUTER_BOUND('',#2884,.T.);
#1862=FACE_OUTER_BOUND('',#2885,.T.);
#1863=FACE_OUTER_BOUND('',#2886,.T.);
#1864=FACE_OUTER_BOUND('',#2887,.T.);
#1865=FACE_OUTER_BOUND('',#2888,.T.);
#1866=FACE_OUTER_BOUND('',#2889,.T.);
#1867=FACE_OUTER_BOUND('',#2890,.T.);
#1868=FACE_OUTER_BOUND('',#2891,.T.);
#1869=FACE_OUTER_BOUND('',#2892,.T.);
#1870=FACE_OUTER_BOUND('',#2893,.T.);
#1871=FACE_OUTER_BOUND('',#2894,.T.);
#1872=FACE_OUTER_BOUND('',#2895,.T.);
#1873=FACE_OUTER_BOUND('',#2896,.T.);
#1874=FACE_OUTER_BOUND('',#2897,.T.);
#1875=FACE_OUTER_BOUND('',#2898,.T.);
#1876=FACE_OUTER_BOUND('',#2899,.T.);
#1877=FACE_OUTER_BOUND('',#2900,.T.);
#1878=FACE_OUTER_BOUND('',#2901,.T.);
#1879=FACE_OUTER_BOUND('',#2903,.T.);
#1880=FACE_OUTER_BOUND('',#2905,.T.);
#1881=FACE_OUTER_BOUND('',#2906,.T.);
#1882=FACE_OUTER_BOUND('',#2907,.T.);
#1883=FACE_OUTER_BOUND('',#2908,.T.);
#1884=FACE_OUTER_BOUND('',#2909,.T.);
#1885=FACE_OUTER_BOUND('',#2910,.T.);
#1886=FACE_OUTER_BOUND('',#2911,.T.);
#1887=FACE_OUTER_BOUND('',#2912,.T.);
#1888=FACE_OUTER_BOUND('',#2913,.T.);
#1889=FACE_OUTER_BOUND('',#2915,.T.);
#1890=FACE_OUTER_BOUND('',#2917,.T.);
#1891=FACE_OUTER_BOUND('',#2918,.T.);
#1892=FACE_OUTER_BOUND('',#2919,.T.);
#1893=FACE_OUTER_BOUND('',#2920,.T.);
#1894=FACE_OUTER_BOUND('',#2921,.T.);
#1895=FACE_OUTER_BOUND('',#2922,.T.);
#1896=FACE_OUTER_BOUND('',#2923,.T.);
#1897=FACE_OUTER_BOUND('',#2924,.T.);
#1898=FACE_OUTER_BOUND('',#2925,.T.);
#1899=FACE_OUTER_BOUND('',#2926,.T.);
#1900=FACE_OUTER_BOUND('',#2927,.T.);
#1901=FACE_OUTER_BOUND('',#2928,.T.);
#1902=FACE_OUTER_BOUND('',#2929,.T.);
#1903=FACE_OUTER_BOUND('',#2930,.T.);
#1904=FACE_OUTER_BOUND('',#2931,.T.);
#1905=FACE_OUTER_BOUND('',#2932,.T.);
#1906=FACE_OUTER_BOUND('',#2933,.T.);
#1907=FACE_OUTER_BOUND('',#2934,.T.);
#1908=FACE_OUTER_BOUND('',#2935,.T.);
#1909=FACE_OUTER_BOUND('',#2936,.T.);
#1910=FACE_OUTER_BOUND('',#2937,.T.);
#1911=FACE_OUTER_BOUND('',#2938,.T.);
#1912=FACE_OUTER_BOUND('',#2939,.T.);
#1913=FACE_OUTER_BOUND('',#2940,.T.);
#1914=FACE_OUTER_BOUND('',#2941,.T.);
#1915=FACE_OUTER_BOUND('',#2942,.T.);
#1916=FACE_OUTER_BOUND('',#2943,.T.);
#1917=FACE_OUTER_BOUND('',#2944,.T.);
#1918=FACE_OUTER_BOUND('',#2945,.T.);
#1919=FACE_OUTER_BOUND('',#2946,.T.);
#1920=FACE_OUTER_BOUND('',#2947,.T.);
#1921=FACE_OUTER_BOUND('',#2948,.T.);
#1922=FACE_OUTER_BOUND('',#2949,.T.);
#1923=FACE_OUTER_BOUND('',#2950,.T.);
#1924=FACE_OUTER_BOUND('',#2952,.T.);
#1925=FACE_OUTER_BOUND('',#2954,.T.);
#1926=FACE_OUTER_BOUND('',#2955,.T.);
#1927=FACE_OUTER_BOUND('',#2956,.T.);
#1928=FACE_OUTER_BOUND('',#2957,.T.);
#1929=FACE_OUTER_BOUND('',#2958,.T.);
#1930=FACE_OUTER_BOUND('',#2959,.T.);
#1931=FACE_OUTER_BOUND('',#2960,.T.);
#1932=FACE_OUTER_BOUND('',#2961,.T.);
#1933=FACE_OUTER_BOUND('',#2962,.T.);
#1934=FACE_OUTER_BOUND('',#2963,.T.);
#1935=FACE_OUTER_BOUND('',#2964,.T.);
#1936=FACE_OUTER_BOUND('',#2965,.T.);
#1937=FACE_OUTER_BOUND('',#2966,.T.);
#1938=FACE_OUTER_BOUND('',#2967,.T.);
#1939=FACE_OUTER_BOUND('',#2968,.T.);
#1940=FACE_OUTER_BOUND('',#2969,.T.);
#1941=FACE_OUTER_BOUND('',#2970,.T.);
#1942=FACE_OUTER_BOUND('',#2971,.T.);
#1943=FACE_OUTER_BOUND('',#2972,.T.);
#1944=FACE_OUTER_BOUND('',#2973,.T.);
#1945=FACE_OUTER_BOUND('',#2974,.T.);
#1946=FACE_OUTER_BOUND('',#2975,.T.);
#1947=FACE_OUTER_BOUND('',#2976,.T.);
#1948=FACE_OUTER_BOUND('',#2977,.T.);
#1949=FACE_OUTER_BOUND('',#2978,.T.);
#1950=FACE_OUTER_BOUND('',#2979,.T.);
#1951=FACE_OUTER_BOUND('',#2980,.T.);
#1952=FACE_OUTER_BOUND('',#2981,.T.);
#1953=FACE_OUTER_BOUND('',#2982,.T.);
#1954=FACE_OUTER_BOUND('',#2983,.T.);
#1955=FACE_OUTER_BOUND('',#2984,.T.);
#1956=FACE_OUTER_BOUND('',#2985,.T.);
#1957=FACE_OUTER_BOUND('',#2986,.T.);
#1958=FACE_OUTER_BOUND('',#2987,.T.);
#1959=FACE_OUTER_BOUND('',#2988,.T.);
#1960=FACE_OUTER_BOUND('',#2989,.T.);
#1961=FACE_OUTER_BOUND('',#2990,.T.);
#1962=FACE_OUTER_BOUND('',#2991,.T.);
#1963=FACE_OUTER_BOUND('',#2992,.T.);
#1964=FACE_OUTER_BOUND('',#2993,.T.);
#1965=FACE_OUTER_BOUND('',#2994,.T.);
#1966=FACE_OUTER_BOUND('',#2995,.T.);
#1967=FACE_OUTER_BOUND('',#2996,.T.);
#1968=FACE_OUTER_BOUND('',#2997,.T.);
#1969=FACE_OUTER_BOUND('',#2998,.T.);
#1970=FACE_OUTER_BOUND('',#2999,.T.);
#1971=FACE_OUTER_BOUND('',#3000,.T.);
#1972=FACE_OUTER_BOUND('',#3001,.T.);
#1973=FACE_OUTER_BOUND('',#3002,.T.);
#1974=FACE_OUTER_BOUND('',#3003,.T.);
#1975=FACE_OUTER_BOUND('',#3004,.T.);
#1976=FACE_OUTER_BOUND('',#3005,.T.);
#1977=FACE_OUTER_BOUND('',#3006,.T.);
#1978=FACE_OUTER_BOUND('',#3007,.T.);
#1979=FACE_OUTER_BOUND('',#3008,.T.);
#1980=FACE_OUTER_BOUND('',#3009,.T.);
#1981=FACE_OUTER_BOUND('',#3010,.T.);
#1982=FACE_OUTER_BOUND('',#3011,.T.);
#1983=FACE_OUTER_BOUND('',#3012,.T.);
#1984=FACE_OUTER_BOUND('',#3013,.T.);
#1985=FACE_OUTER_BOUND('',#3014,.T.);
#1986=FACE_OUTER_BOUND('',#3015,.T.);
#1987=FACE_OUTER_BOUND('',#3016,.T.);
#1988=FACE_OUTER_BOUND('',#3019,.T.);
#1989=FACE_OUTER_BOUND('',#3020,.T.);
#1990=FACE_OUTER_BOUND('',#3021,.T.);
#1991=FACE_OUTER_BOUND('',#3022,.T.);
#1992=FACE_OUTER_BOUND('',#3025,.T.);
#1993=FACE_OUTER_BOUND('',#3027,.T.);
#1994=FACE_OUTER_BOUND('',#3029,.T.);
#1995=FACE_OUTER_BOUND('',#3030,.T.);
#1996=FACE_OUTER_BOUND('',#3031,.T.);
#1997=FACE_OUTER_BOUND('',#3033,.T.);
#1998=FACE_OUTER_BOUND('',#3034,.T.);
#1999=FACE_OUTER_BOUND('',#3035,.T.);
#2000=FACE_OUTER_BOUND('',#3036,.T.);
#2001=FACE_OUTER_BOUND('',#3037,.T.);
#2002=FACE_OUTER_BOUND('',#3038,.T.);
#2003=FACE_OUTER_BOUND('',#3039,.T.);
#2004=FACE_OUTER_BOUND('',#3040,.T.);
#2005=FACE_OUTER_BOUND('',#3042,.T.);
#2006=FACE_OUTER_BOUND('',#3043,.T.);
#2007=FACE_OUTER_BOUND('',#3044,.T.);
#2008=FACE_OUTER_BOUND('',#3045,.T.);
#2009=FACE_OUTER_BOUND('',#3046,.T.);
#2010=FACE_OUTER_BOUND('',#3048,.T.);
#2011=FACE_OUTER_BOUND('',#3049,.T.);
#2012=FACE_OUTER_BOUND('',#3050,.T.);
#2013=FACE_OUTER_BOUND('',#3051,.T.);
#2014=FACE_OUTER_BOUND('',#3052,.T.);
#2015=FACE_OUTER_BOUND('',#3053,.T.);
#2016=FACE_OUTER_BOUND('',#3054,.T.);
#2017=FACE_OUTER_BOUND('',#3055,.T.);
#2018=FACE_OUTER_BOUND('',#3056,.T.);
#2019=FACE_OUTER_BOUND('',#3057,.T.);
#2020=FACE_OUTER_BOUND('',#3058,.T.);
#2021=FACE_OUTER_BOUND('',#3059,.T.);
#2022=FACE_OUTER_BOUND('',#3060,.T.);
#2023=FACE_OUTER_BOUND('',#3061,.T.);
#2024=FACE_OUTER_BOUND('',#3062,.T.);
#2025=FACE_OUTER_BOUND('',#3063,.T.);
#2026=FACE_OUTER_BOUND('',#3064,.T.);
#2027=FACE_OUTER_BOUND('',#3065,.T.);
#2028=FACE_OUTER_BOUND('',#3066,.T.);
#2029=FACE_OUTER_BOUND('',#3067,.T.);
#2030=FACE_OUTER_BOUND('',#3068,.T.);
#2031=FACE_OUTER_BOUND('',#3069,.T.);
#2032=FACE_OUTER_BOUND('',#3070,.T.);
#2033=FACE_OUTER_BOUND('',#3071,.T.);
#2034=FACE_OUTER_BOUND('',#3072,.T.);
#2035=FACE_OUTER_BOUND('',#3073,.T.);
#2036=FACE_OUTER_BOUND('',#3074,.T.);
#2037=FACE_OUTER_BOUND('',#3075,.T.);
#2038=FACE_OUTER_BOUND('',#3076,.T.);
#2039=FACE_OUTER_BOUND('',#3077,.T.);
#2040=FACE_OUTER_BOUND('',#3078,.T.);
#2041=FACE_OUTER_BOUND('',#3079,.T.);
#2042=FACE_OUTER_BOUND('',#3080,.T.);
#2043=FACE_OUTER_BOUND('',#3081,.T.);
#2044=FACE_OUTER_BOUND('',#3082,.T.);
#2045=FACE_OUTER_BOUND('',#3083,.T.);
#2046=FACE_OUTER_BOUND('',#3084,.T.);
#2047=FACE_OUTER_BOUND('',#3085,.T.);
#2048=FACE_OUTER_BOUND('',#3086,.T.);
#2049=FACE_OUTER_BOUND('',#3087,.T.);
#2050=FACE_OUTER_BOUND('',#3088,.T.);
#2051=FACE_OUTER_BOUND('',#3089,.T.);
#2052=FACE_OUTER_BOUND('',#3090,.T.);
#2053=FACE_OUTER_BOUND('',#3091,.T.);
#2054=FACE_OUTER_BOUND('',#3092,.T.);
#2055=FACE_OUTER_BOUND('',#3093,.T.);
#2056=FACE_OUTER_BOUND('',#3094,.T.);
#2057=FACE_OUTER_BOUND('',#3095,.T.);
#2058=FACE_OUTER_BOUND('',#3096,.T.);
#2059=FACE_OUTER_BOUND('',#3097,.T.);
#2060=FACE_OUTER_BOUND('',#3099,.T.);
#2061=FACE_OUTER_BOUND('',#3101,.T.);
#2062=FACE_OUTER_BOUND('',#3102,.T.);
#2063=FACE_OUTER_BOUND('',#3104,.T.);
#2064=FACE_OUTER_BOUND('',#3105,.T.);
#2065=FACE_OUTER_BOUND('',#3106,.T.);
#2066=FACE_OUTER_BOUND('',#3108,.T.);
#2067=FACE_OUTER_BOUND('',#3110,.T.);
#2068=FACE_OUTER_BOUND('',#3112,.T.);
#2069=FACE_OUTER_BOUND('',#3113,.T.);
#2070=FACE_OUTER_BOUND('',#3115,.T.);
#2071=FACE_OUTER_BOUND('',#3117,.T.);
#2072=FACE_OUTER_BOUND('',#3118,.T.);
#2073=FACE_OUTER_BOUND('',#3119,.T.);
#2074=FACE_OUTER_BOUND('',#3121,.T.);
#2075=FACE_OUTER_BOUND('',#3122,.T.);
#2076=FACE_OUTER_BOUND('',#3123,.T.);
#2077=FACE_OUTER_BOUND('',#3124,.T.);
#2078=FACE_OUTER_BOUND('',#3125,.T.);
#2079=FACE_OUTER_BOUND('',#3126,.T.);
#2080=FACE_OUTER_BOUND('',#3127,.T.);
#2081=FACE_OUTER_BOUND('',#3128,.T.);
#2082=FACE_OUTER_BOUND('',#3129,.T.);
#2083=FACE_OUTER_BOUND('',#3130,.T.);
#2084=FACE_OUTER_BOUND('',#3131,.T.);
#2085=FACE_OUTER_BOUND('',#3132,.T.);
#2086=FACE_OUTER_BOUND('',#3133,.T.);
#2087=FACE_OUTER_BOUND('',#3134,.T.);
#2088=FACE_OUTER_BOUND('',#3135,.T.);
#2089=FACE_OUTER_BOUND('',#3136,.T.);
#2090=FACE_OUTER_BOUND('',#3137,.T.);
#2091=FACE_OUTER_BOUND('',#3138,.T.);
#2092=FACE_OUTER_BOUND('',#3139,.T.);
#2093=FACE_OUTER_BOUND('',#3140,.T.);
#2094=FACE_OUTER_BOUND('',#3141,.T.);
#2095=FACE_OUTER_BOUND('',#3142,.T.);
#2096=FACE_OUTER_BOUND('',#3143,.T.);
#2097=FACE_OUTER_BOUND('',#3144,.T.);
#2098=FACE_OUTER_BOUND('',#3145,.T.);
#2099=FACE_OUTER_BOUND('',#3146,.T.);
#2100=FACE_OUTER_BOUND('',#3147,.T.);
#2101=FACE_OUTER_BOUND('',#3148,.T.);
#2102=FACE_OUTER_BOUND('',#3149,.T.);
#2103=FACE_OUTER_BOUND('',#3150,.T.);
#2104=FACE_OUTER_BOUND('',#3151,.T.);
#2105=FACE_OUTER_BOUND('',#3152,.T.);
#2106=FACE_OUTER_BOUND('',#3153,.T.);
#2107=FACE_OUTER_BOUND('',#3154,.T.);
#2108=FACE_OUTER_BOUND('',#3155,.T.);
#2109=FACE_OUTER_BOUND('',#3156,.T.);
#2110=FACE_OUTER_BOUND('',#3157,.T.);
#2111=FACE_OUTER_BOUND('',#3158,.T.);
#2112=FACE_OUTER_BOUND('',#3159,.T.);
#2113=FACE_OUTER_BOUND('',#3160,.T.);
#2114=FACE_OUTER_BOUND('',#3161,.T.);
#2115=FACE_OUTER_BOUND('',#3162,.T.);
#2116=FACE_OUTER_BOUND('',#3163,.T.);
#2117=FACE_OUTER_BOUND('',#3164,.T.);
#2118=FACE_OUTER_BOUND('',#3165,.T.);
#2119=FACE_OUTER_BOUND('',#3166,.T.);
#2120=FACE_OUTER_BOUND('',#3167,.T.);
#2121=FACE_OUTER_BOUND('',#3168,.T.);
#2122=FACE_OUTER_BOUND('',#3169,.T.);
#2123=FACE_OUTER_BOUND('',#3170,.T.);
#2124=FACE_OUTER_BOUND('',#3171,.T.);
#2125=FACE_OUTER_BOUND('',#3172,.T.);
#2126=FACE_OUTER_BOUND('',#3173,.T.);
#2127=FACE_OUTER_BOUND('',#3174,.T.);
#2128=FACE_OUTER_BOUND('',#3175,.T.);
#2129=FACE_OUTER_BOUND('',#3176,.T.);
#2130=FACE_OUTER_BOUND('',#3177,.T.);
#2131=FACE_OUTER_BOUND('',#3178,.T.);
#2132=FACE_OUTER_BOUND('',#3179,.T.);
#2133=FACE_OUTER_BOUND('',#3180,.T.);
#2134=FACE_OUTER_BOUND('',#3181,.T.);
#2135=FACE_OUTER_BOUND('',#3182,.T.);
#2136=FACE_OUTER_BOUND('',#3183,.T.);
#2137=FACE_OUTER_BOUND('',#3184,.T.);
#2138=FACE_OUTER_BOUND('',#3185,.T.);
#2139=FACE_OUTER_BOUND('',#3186,.T.);
#2140=FACE_OUTER_BOUND('',#3187,.T.);
#2141=FACE_OUTER_BOUND('',#3188,.T.);
#2142=FACE_OUTER_BOUND('',#3189,.T.);
#2143=FACE_OUTER_BOUND('',#3190,.T.);
#2144=FACE_OUTER_BOUND('',#3191,.T.);
#2145=FACE_OUTER_BOUND('',#3192,.T.);
#2146=FACE_OUTER_BOUND('',#3193,.T.);
#2147=FACE_OUTER_BOUND('',#3194,.T.);
#2148=FACE_OUTER_BOUND('',#3195,.T.);
#2149=FACE_OUTER_BOUND('',#3196,.T.);
#2150=FACE_OUTER_BOUND('',#3197,.T.);
#2151=FACE_OUTER_BOUND('',#3198,.T.);
#2152=FACE_OUTER_BOUND('',#3199,.T.);
#2153=FACE_OUTER_BOUND('',#3200,.T.);
#2154=FACE_OUTER_BOUND('',#3201,.T.);
#2155=FACE_OUTER_BOUND('',#3202,.T.);
#2156=FACE_OUTER_BOUND('',#3203,.T.);
#2157=FACE_OUTER_BOUND('',#3204,.T.);
#2158=FACE_OUTER_BOUND('',#3205,.T.);
#2159=FACE_OUTER_BOUND('',#3206,.T.);
#2160=FACE_OUTER_BOUND('',#3207,.T.);
#2161=FACE_OUTER_BOUND('',#3208,.T.);
#2162=FACE_OUTER_BOUND('',#3209,.T.);
#2163=FACE_OUTER_BOUND('',#3210,.T.);
#2164=FACE_OUTER_BOUND('',#3211,.T.);
#2165=FACE_OUTER_BOUND('',#3212,.T.);
#2166=FACE_OUTER_BOUND('',#3213,.T.);
#2167=FACE_OUTER_BOUND('',#3214,.T.);
#2168=FACE_OUTER_BOUND('',#3215,.T.);
#2169=FACE_OUTER_BOUND('',#3216,.T.);
#2170=FACE_OUTER_BOUND('',#3217,.T.);
#2171=FACE_OUTER_BOUND('',#3218,.T.);
#2172=FACE_OUTER_BOUND('',#3219,.T.);
#2173=FACE_OUTER_BOUND('',#3220,.T.);
#2174=FACE_OUTER_BOUND('',#3221,.T.);
#2175=FACE_OUTER_BOUND('',#3222,.T.);
#2176=FACE_OUTER_BOUND('',#3223,.T.);
#2177=FACE_OUTER_BOUND('',#3224,.T.);
#2178=FACE_OUTER_BOUND('',#3225,.T.);
#2179=FACE_OUTER_BOUND('',#3226,.T.);
#2180=FACE_OUTER_BOUND('',#3227,.T.);
#2181=FACE_OUTER_BOUND('',#3228,.T.);
#2182=FACE_OUTER_BOUND('',#3229,.T.);
#2183=FACE_OUTER_BOUND('',#3230,.T.);
#2184=FACE_OUTER_BOUND('',#3231,.T.);
#2185=FACE_OUTER_BOUND('',#3232,.T.);
#2186=FACE_OUTER_BOUND('',#3233,.T.);
#2187=FACE_OUTER_BOUND('',#3234,.T.);
#2188=FACE_OUTER_BOUND('',#3235,.T.);
#2189=FACE_OUTER_BOUND('',#3236,.T.);
#2190=FACE_OUTER_BOUND('',#3237,.T.);
#2191=FACE_OUTER_BOUND('',#3238,.T.);
#2192=FACE_OUTER_BOUND('',#3239,.T.);
#2193=FACE_OUTER_BOUND('',#3240,.T.);
#2194=FACE_OUTER_BOUND('',#3241,.T.);
#2195=FACE_OUTER_BOUND('',#3242,.T.);
#2196=FACE_OUTER_BOUND('',#3243,.T.);
#2197=FACE_OUTER_BOUND('',#3244,.T.);
#2198=FACE_OUTER_BOUND('',#3245,.T.);
#2199=FACE_OUTER_BOUND('',#3246,.T.);
#2200=FACE_OUTER_BOUND('',#3247,.T.);
#2201=FACE_OUTER_BOUND('',#3249,.T.);
#2202=FACE_OUTER_BOUND('',#3250,.T.);
#2203=FACE_OUTER_BOUND('',#3251,.T.);
#2204=FACE_OUTER_BOUND('',#3252,.T.);
#2205=FACE_OUTER_BOUND('',#3253,.T.);
#2206=FACE_OUTER_BOUND('',#3254,.T.);
#2207=FACE_OUTER_BOUND('',#3255,.T.);
#2208=FACE_OUTER_BOUND('',#3256,.T.);
#2209=FACE_OUTER_BOUND('',#3257,.T.);
#2210=FACE_OUTER_BOUND('',#3258,.T.);
#2211=FACE_OUTER_BOUND('',#3259,.T.);
#2212=FACE_OUTER_BOUND('',#3260,.T.);
#2213=FACE_OUTER_BOUND('',#3261,.T.);
#2214=FACE_OUTER_BOUND('',#3262,.T.);
#2215=FACE_OUTER_BOUND('',#3263,.T.);
#2216=FACE_OUTER_BOUND('',#3264,.T.);
#2217=FACE_OUTER_BOUND('',#3265,.T.);
#2218=FACE_OUTER_BOUND('',#3266,.T.);
#2219=FACE_OUTER_BOUND('',#3267,.T.);
#2220=FACE_OUTER_BOUND('',#3268,.T.);
#2221=FACE_OUTER_BOUND('',#3269,.T.);
#2222=FACE_OUTER_BOUND('',#3270,.T.);
#2223=FACE_OUTER_BOUND('',#3271,.T.);
#2224=FACE_OUTER_BOUND('',#3272,.T.);
#2225=FACE_OUTER_BOUND('',#3273,.T.);
#2226=FACE_OUTER_BOUND('',#3274,.T.);
#2227=FACE_OUTER_BOUND('',#3275,.T.);
#2228=FACE_OUTER_BOUND('',#3276,.T.);
#2229=FACE_OUTER_BOUND('',#3277,.T.);
#2230=FACE_OUTER_BOUND('',#3278,.T.);
#2231=FACE_OUTER_BOUND('',#3279,.T.);
#2232=FACE_OUTER_BOUND('',#3280,.T.);
#2233=FACE_OUTER_BOUND('',#3281,.T.);
#2234=FACE_OUTER_BOUND('',#3282,.T.);
#2235=FACE_OUTER_BOUND('',#3283,.T.);
#2236=FACE_OUTER_BOUND('',#3284,.T.);
#2237=FACE_OUTER_BOUND('',#3285,.T.);
#2238=FACE_OUTER_BOUND('',#3286,.T.);
#2239=FACE_OUTER_BOUND('',#3287,.T.);
#2240=FACE_OUTER_BOUND('',#3288,.T.);
#2241=FACE_OUTER_BOUND('',#3289,.T.);
#2242=FACE_OUTER_BOUND('',#3290,.T.);
#2243=FACE_OUTER_BOUND('',#3291,.T.);
#2244=FACE_OUTER_BOUND('',#3292,.T.);
#2245=FACE_OUTER_BOUND('',#3293,.T.);
#2246=FACE_OUTER_BOUND('',#3294,.T.);
#2247=FACE_OUTER_BOUND('',#3295,.T.);
#2248=FACE_OUTER_BOUND('',#3296,.T.);
#2249=FACE_OUTER_BOUND('',#3297,.T.);
#2250=FACE_OUTER_BOUND('',#3298,.T.);
#2251=FACE_OUTER_BOUND('',#3299,.T.);
#2252=FACE_OUTER_BOUND('',#3300,.T.);
#2253=FACE_OUTER_BOUND('',#3301,.T.);
#2254=FACE_OUTER_BOUND('',#3302,.T.);
#2255=FACE_OUTER_BOUND('',#3303,.T.);
#2256=FACE_OUTER_BOUND('',#3304,.T.);
#2257=FACE_OUTER_BOUND('',#3305,.T.);
#2258=FACE_OUTER_BOUND('',#3306,.T.);
#2259=FACE_OUTER_BOUND('',#3307,.T.);
#2260=FACE_OUTER_BOUND('',#3308,.T.);
#2261=FACE_OUTER_BOUND('',#3309,.T.);
#2262=FACE_OUTER_BOUND('',#3310,.T.);
#2263=FACE_OUTER_BOUND('',#3311,.T.);
#2264=FACE_OUTER_BOUND('',#3312,.T.);
#2265=FACE_OUTER_BOUND('',#3313,.T.);
#2266=FACE_OUTER_BOUND('',#3314,.T.);
#2267=FACE_OUTER_BOUND('',#3315,.T.);
#2268=FACE_OUTER_BOUND('',#3316,.T.);
#2269=FACE_OUTER_BOUND('',#3317,.T.);
#2270=FACE_OUTER_BOUND('',#3318,.T.);
#2271=FACE_OUTER_BOUND('',#3319,.T.);
#2272=FACE_OUTER_BOUND('',#3320,.T.);
#2273=FACE_OUTER_BOUND('',#3321,.T.);
#2274=FACE_OUTER_BOUND('',#3322,.T.);
#2275=FACE_OUTER_BOUND('',#3323,.T.);
#2276=FACE_OUTER_BOUND('',#3324,.T.);
#2277=FACE_OUTER_BOUND('',#3325,.T.);
#2278=FACE_OUTER_BOUND('',#3326,.T.);
#2279=FACE_OUTER_BOUND('',#3327,.T.);
#2280=FACE_OUTER_BOUND('',#3328,.T.);
#2281=FACE_OUTER_BOUND('',#3329,.T.);
#2282=FACE_OUTER_BOUND('',#3330,.T.);
#2283=FACE_OUTER_BOUND('',#3331,.T.);
#2284=FACE_OUTER_BOUND('',#3332,.T.);
#2285=FACE_OUTER_BOUND('',#3333,.T.);
#2286=FACE_OUTER_BOUND('',#3334,.T.);
#2287=FACE_OUTER_BOUND('',#3335,.T.);
#2288=FACE_OUTER_BOUND('',#3336,.T.);
#2289=FACE_OUTER_BOUND('',#3337,.T.);
#2290=FACE_OUTER_BOUND('',#3338,.T.);
#2291=FACE_OUTER_BOUND('',#3339,.T.);
#2292=FACE_OUTER_BOUND('',#3340,.T.);
#2293=FACE_OUTER_BOUND('',#3341,.T.);
#2294=FACE_OUTER_BOUND('',#3342,.T.);
#2295=FACE_OUTER_BOUND('',#3343,.T.);
#2296=FACE_OUTER_BOUND('',#3344,.T.);
#2297=FACE_OUTER_BOUND('',#3345,.T.);
#2298=FACE_OUTER_BOUND('',#3346,.T.);
#2299=FACE_OUTER_BOUND('',#3347,.T.);
#2300=FACE_OUTER_BOUND('',#3348,.T.);
#2301=FACE_OUTER_BOUND('',#3349,.T.);
#2302=FACE_OUTER_BOUND('',#3350,.T.);
#2303=FACE_OUTER_BOUND('',#3351,.T.);
#2304=FACE_OUTER_BOUND('',#3352,.T.);
#2305=FACE_OUTER_BOUND('',#3353,.T.);
#2306=FACE_OUTER_BOUND('',#3354,.T.);
#2307=FACE_OUTER_BOUND('',#3355,.T.);
#2308=FACE_OUTER_BOUND('',#3356,.T.);
#2309=FACE_OUTER_BOUND('',#3357,.T.);
#2310=FACE_OUTER_BOUND('',#3358,.T.);
#2311=FACE_OUTER_BOUND('',#3359,.T.);
#2312=FACE_OUTER_BOUND('',#3360,.T.);
#2313=FACE_OUTER_BOUND('',#3361,.T.);
#2314=FACE_OUTER_BOUND('',#3362,.T.);
#2315=FACE_OUTER_BOUND('',#3363,.T.);
#2316=FACE_OUTER_BOUND('',#3364,.T.);
#2317=FACE_OUTER_BOUND('',#3365,.T.);
#2318=FACE_OUTER_BOUND('',#3366,.T.);
#2319=FACE_OUTER_BOUND('',#3367,.T.);
#2320=FACE_OUTER_BOUND('',#3368,.T.);
#2321=FACE_OUTER_BOUND('',#3369,.T.);
#2322=FACE_OUTER_BOUND('',#3370,.T.);
#2323=FACE_OUTER_BOUND('',#3371,.T.);
#2324=FACE_OUTER_BOUND('',#3372,.T.);
#2325=FACE_OUTER_BOUND('',#3373,.T.);
#2326=FACE_OUTER_BOUND('',#3374,.T.);
#2327=FACE_OUTER_BOUND('',#3375,.T.);
#2328=FACE_OUTER_BOUND('',#3376,.T.);
#2329=FACE_OUTER_BOUND('',#3377,.T.);
#2330=FACE_OUTER_BOUND('',#3378,.T.);
#2331=FACE_OUTER_BOUND('',#3379,.T.);
#2332=FACE_OUTER_BOUND('',#3380,.T.);
#2333=FACE_OUTER_BOUND('',#3381,.T.);
#2334=FACE_OUTER_BOUND('',#3382,.T.);
#2335=FACE_OUTER_BOUND('',#3383,.T.);
#2336=FACE_OUTER_BOUND('',#3384,.T.);
#2337=FACE_OUTER_BOUND('',#3385,.T.);
#2338=FACE_OUTER_BOUND('',#3386,.T.);
#2339=FACE_OUTER_BOUND('',#3387,.T.);
#2340=FACE_OUTER_BOUND('',#3388,.T.);
#2341=FACE_OUTER_BOUND('',#3389,.T.);
#2342=FACE_OUTER_BOUND('',#3390,.T.);
#2343=FACE_OUTER_BOUND('',#3391,.T.);
#2344=FACE_OUTER_BOUND('',#3392,.T.);
#2345=FACE_OUTER_BOUND('',#3393,.T.);
#2346=FACE_OUTER_BOUND('',#3394,.T.);
#2347=FACE_OUTER_BOUND('',#3395,.T.);
#2348=FACE_OUTER_BOUND('',#3396,.T.);
#2349=FACE_OUTER_BOUND('',#3397,.T.);
#2350=FACE_OUTER_BOUND('',#3398,.T.);
#2351=FACE_OUTER_BOUND('',#3399,.T.);
#2352=FACE_OUTER_BOUND('',#3400,.T.);
#2353=FACE_OUTER_BOUND('',#3401,.T.);
#2354=FACE_OUTER_BOUND('',#3402,.T.);
#2355=FACE_OUTER_BOUND('',#3403,.T.);
#2356=FACE_OUTER_BOUND('',#3404,.T.);
#2357=FACE_OUTER_BOUND('',#3405,.T.);
#2358=FACE_OUTER_BOUND('',#3406,.T.);
#2359=FACE_OUTER_BOUND('',#3407,.T.);
#2360=FACE_OUTER_BOUND('',#3408,.T.);
#2361=FACE_OUTER_BOUND('',#3409,.T.);
#2362=FACE_OUTER_BOUND('',#3410,.T.);
#2363=FACE_OUTER_BOUND('',#3411,.T.);
#2364=FACE_OUTER_BOUND('',#3412,.T.);
#2365=FACE_OUTER_BOUND('',#3414,.T.);
#2366=FACE_OUTER_BOUND('',#3415,.T.);
#2367=FACE_OUTER_BOUND('',#3416,.T.);
#2368=FACE_OUTER_BOUND('',#3417,.T.);
#2369=FACE_OUTER_BOUND('',#3418,.T.);
#2370=FACE_OUTER_BOUND('',#3419,.T.);
#2371=FACE_OUTER_BOUND('',#3420,.T.);
#2372=FACE_OUTER_BOUND('',#3421,.T.);
#2373=FACE_OUTER_BOUND('',#3422,.T.);
#2374=FACE_OUTER_BOUND('',#3423,.T.);
#2375=FACE_OUTER_BOUND('',#3424,.T.);
#2376=FACE_OUTER_BOUND('',#3425,.T.);
#2377=FACE_OUTER_BOUND('',#3426,.T.);
#2378=FACE_OUTER_BOUND('',#3427,.T.);
#2379=FACE_OUTER_BOUND('',#3428,.T.);
#2380=FACE_OUTER_BOUND('',#3429,.T.);
#2381=FACE_OUTER_BOUND('',#3430,.T.);
#2382=FACE_OUTER_BOUND('',#3431,.T.);
#2383=FACE_OUTER_BOUND('',#3432,.T.);
#2384=FACE_OUTER_BOUND('',#3433,.T.);
#2385=FACE_OUTER_BOUND('',#3434,.T.);
#2386=FACE_OUTER_BOUND('',#3435,.T.);
#2387=FACE_OUTER_BOUND('',#3436,.T.);
#2388=FACE_OUTER_BOUND('',#3437,.T.);
#2389=FACE_OUTER_BOUND('',#3438,.T.);
#2390=FACE_OUTER_BOUND('',#3439,.T.);
#2391=FACE_OUTER_BOUND('',#3440,.T.);
#2392=FACE_OUTER_BOUND('',#3441,.T.);
#2393=FACE_OUTER_BOUND('',#3442,.T.);
#2394=FACE_OUTER_BOUND('',#3443,.T.);
#2395=FACE_OUTER_BOUND('',#3444,.T.);
#2396=FACE_OUTER_BOUND('',#3445,.T.);
#2397=FACE_OUTER_BOUND('',#3446,.T.);
#2398=FACE_OUTER_BOUND('',#3447,.T.);
#2399=FACE_OUTER_BOUND('',#3448,.T.);
#2400=FACE_OUTER_BOUND('',#3449,.T.);
#2401=FACE_OUTER_BOUND('',#3450,.T.);
#2402=FACE_OUTER_BOUND('',#3451,.T.);
#2403=FACE_OUTER_BOUND('',#3452,.T.);
#2404=FACE_OUTER_BOUND('',#3453,.T.);
#2405=FACE_OUTER_BOUND('',#3454,.T.);
#2406=FACE_OUTER_BOUND('',#3455,.T.);
#2407=FACE_OUTER_BOUND('',#3456,.T.);
#2408=FACE_OUTER_BOUND('',#3457,.T.);
#2409=FACE_OUTER_BOUND('',#3458,.T.);
#2410=FACE_OUTER_BOUND('',#3459,.T.);
#2411=FACE_OUTER_BOUND('',#3460,.T.);
#2412=FACE_OUTER_BOUND('',#3461,.T.);
#2413=FACE_OUTER_BOUND('',#3462,.T.);
#2414=FACE_OUTER_BOUND('',#3463,.T.);
#2415=FACE_OUTER_BOUND('',#3464,.T.);
#2416=FACE_OUTER_BOUND('',#3465,.T.);
#2417=FACE_OUTER_BOUND('',#3466,.T.);
#2418=FACE_OUTER_BOUND('',#3467,.T.);
#2419=FACE_OUTER_BOUND('',#3468,.T.);
#2420=FACE_OUTER_BOUND('',#3469,.T.);
#2421=FACE_OUTER_BOUND('',#3470,.T.);
#2422=FACE_OUTER_BOUND('',#3471,.T.);
#2423=FACE_OUTER_BOUND('',#3472,.T.);
#2424=FACE_OUTER_BOUND('',#3473,.T.);
#2425=FACE_OUTER_BOUND('',#3474,.T.);
#2426=FACE_OUTER_BOUND('',#3475,.T.);
#2427=FACE_OUTER_BOUND('',#3476,.T.);
#2428=FACE_OUTER_BOUND('',#3477,.T.);
#2429=FACE_OUTER_BOUND('',#3478,.T.);
#2430=FACE_OUTER_BOUND('',#3479,.T.);
#2431=FACE_OUTER_BOUND('',#3480,.T.);
#2432=FACE_OUTER_BOUND('',#3481,.T.);
#2433=FACE_OUTER_BOUND('',#3482,.T.);
#2434=FACE_OUTER_BOUND('',#3483,.T.);
#2435=FACE_OUTER_BOUND('',#3484,.T.);
#2436=FACE_OUTER_BOUND('',#3485,.T.);
#2437=FACE_OUTER_BOUND('',#3486,.T.);
#2438=FACE_OUTER_BOUND('',#3487,.T.);
#2439=FACE_OUTER_BOUND('',#3488,.T.);
#2440=FACE_OUTER_BOUND('',#3489,.T.);
#2441=FACE_OUTER_BOUND('',#3490,.T.);
#2442=FACE_OUTER_BOUND('',#3491,.T.);
#2443=FACE_OUTER_BOUND('',#3492,.T.);
#2444=FACE_OUTER_BOUND('',#3493,.T.);
#2445=FACE_OUTER_BOUND('',#3494,.T.);
#2446=FACE_OUTER_BOUND('',#3495,.T.);
#2447=FACE_OUTER_BOUND('',#3496,.T.);
#2448=FACE_OUTER_BOUND('',#3497,.T.);
#2449=FACE_OUTER_BOUND('',#3498,.T.);
#2450=FACE_OUTER_BOUND('',#3499,.T.);
#2451=FACE_OUTER_BOUND('',#3500,.T.);
#2452=FACE_OUTER_BOUND('',#3501,.T.);
#2453=FACE_OUTER_BOUND('',#3502,.T.);
#2454=FACE_OUTER_BOUND('',#3503,.T.);
#2455=FACE_OUTER_BOUND('',#3504,.T.);
#2456=FACE_OUTER_BOUND('',#3505,.T.);
#2457=FACE_OUTER_BOUND('',#3506,.T.);
#2458=FACE_OUTER_BOUND('',#3507,.T.);
#2459=FACE_OUTER_BOUND('',#3508,.T.);
#2460=FACE_OUTER_BOUND('',#3509,.T.);
#2461=FACE_OUTER_BOUND('',#3510,.T.);
#2462=FACE_OUTER_BOUND('',#3511,.T.);
#2463=FACE_OUTER_BOUND('',#3512,.T.);
#2464=FACE_OUTER_BOUND('',#3513,.T.);
#2465=FACE_OUTER_BOUND('',#3514,.T.);
#2466=FACE_OUTER_BOUND('',#3515,.T.);
#2467=FACE_OUTER_BOUND('',#3516,.T.);
#2468=FACE_OUTER_BOUND('',#3517,.T.);
#2469=FACE_OUTER_BOUND('',#3518,.T.);
#2470=FACE_OUTER_BOUND('',#3519,.T.);
#2471=FACE_OUTER_BOUND('',#3520,.T.);
#2472=FACE_OUTER_BOUND('',#3521,.T.);
#2473=FACE_OUTER_BOUND('',#3522,.T.);
#2474=FACE_OUTER_BOUND('',#3523,.T.);
#2475=FACE_OUTER_BOUND('',#3524,.T.);
#2476=FACE_OUTER_BOUND('',#3525,.T.);
#2477=FACE_OUTER_BOUND('',#3526,.T.);
#2478=FACE_OUTER_BOUND('',#3527,.T.);
#2479=FACE_OUTER_BOUND('',#3528,.T.);
#2480=FACE_OUTER_BOUND('',#3529,.T.);
#2481=FACE_OUTER_BOUND('',#3530,.T.);
#2482=FACE_OUTER_BOUND('',#3531,.T.);
#2483=FACE_OUTER_BOUND('',#3532,.T.);
#2484=FACE_OUTER_BOUND('',#3533,.T.);
#2485=FACE_OUTER_BOUND('',#3534,.T.);
#2486=FACE_OUTER_BOUND('',#3535,.T.);
#2487=FACE_OUTER_BOUND('',#3536,.T.);
#2488=FACE_OUTER_BOUND('',#3537,.T.);
#2489=FACE_OUTER_BOUND('',#3538,.T.);
#2490=FACE_OUTER_BOUND('',#3539,.T.);
#2491=FACE_OUTER_BOUND('',#3541,.T.);
#2492=FACE_OUTER_BOUND('',#3543,.T.);
#2493=FACE_OUTER_BOUND('',#3544,.T.);
#2494=FACE_OUTER_BOUND('',#3545,.T.);
#2495=FACE_OUTER_BOUND('',#3546,.T.);
#2496=FACE_OUTER_BOUND('',#3547,.T.);
#2497=FACE_OUTER_BOUND('',#3548,.T.);
#2498=FACE_OUTER_BOUND('',#3549,.T.);
#2499=FACE_OUTER_BOUND('',#3550,.T.);
#2500=FACE_OUTER_BOUND('',#3551,.T.);
#2501=FACE_OUTER_BOUND('',#3552,.T.);
#2502=FACE_OUTER_BOUND('',#3553,.T.);
#2503=FACE_OUTER_BOUND('',#3554,.T.);
#2504=FACE_OUTER_BOUND('',#3555,.T.);
#2505=FACE_OUTER_BOUND('',#3556,.T.);
#2506=FACE_OUTER_BOUND('',#3557,.T.);
#2507=FACE_OUTER_BOUND('',#3558,.T.);
#2508=FACE_OUTER_BOUND('',#3559,.T.);
#2509=FACE_OUTER_BOUND('',#3560,.T.);
#2510=FACE_OUTER_BOUND('',#3561,.T.);
#2511=FACE_OUTER_BOUND('',#3562,.T.);
#2512=FACE_OUTER_BOUND('',#3563,.T.);
#2513=FACE_OUTER_BOUND('',#3564,.T.);
#2514=FACE_OUTER_BOUND('',#3565,.T.);
#2515=FACE_OUTER_BOUND('',#3566,.T.);
#2516=FACE_OUTER_BOUND('',#3567,.T.);
#2517=FACE_OUTER_BOUND('',#3568,.T.);
#2518=FACE_OUTER_BOUND('',#3569,.T.);
#2519=FACE_OUTER_BOUND('',#3570,.T.);
#2520=FACE_OUTER_BOUND('',#3571,.T.);
#2521=FACE_OUTER_BOUND('',#3572,.T.);
#2522=FACE_OUTER_BOUND('',#3573,.T.);
#2523=FACE_OUTER_BOUND('',#3574,.T.);
#2524=FACE_OUTER_BOUND('',#3575,.T.);
#2525=FACE_OUTER_BOUND('',#3576,.T.);
#2526=FACE_OUTER_BOUND('',#3577,.T.);
#2527=FACE_OUTER_BOUND('',#3578,.T.);
#2528=FACE_OUTER_BOUND('',#3579,.T.);
#2529=FACE_OUTER_BOUND('',#3580,.T.);
#2530=FACE_OUTER_BOUND('',#3581,.T.);
#2531=FACE_OUTER_BOUND('',#3582,.T.);
#2532=FACE_OUTER_BOUND('',#3583,.T.);
#2533=FACE_OUTER_BOUND('',#3584,.T.);
#2534=FACE_OUTER_BOUND('',#3585,.T.);
#2535=FACE_OUTER_BOUND('',#3586,.T.);
#2536=FACE_OUTER_BOUND('',#3587,.T.);
#2537=FACE_OUTER_BOUND('',#3588,.T.);
#2538=FACE_OUTER_BOUND('',#3589,.T.);
#2539=FACE_OUTER_BOUND('',#3590,.T.);
#2540=FACE_OUTER_BOUND('',#3591,.T.);
#2541=FACE_OUTER_BOUND('',#3592,.T.);
#2542=FACE_OUTER_BOUND('',#3593,.T.);
#2543=FACE_OUTER_BOUND('',#3594,.T.);
#2544=FACE_OUTER_BOUND('',#3595,.T.);
#2545=FACE_OUTER_BOUND('',#3596,.T.);
#2546=FACE_OUTER_BOUND('',#3597,.T.);
#2547=FACE_OUTER_BOUND('',#3598,.T.);
#2548=FACE_OUTER_BOUND('',#3599,.T.);
#2549=FACE_OUTER_BOUND('',#3600,.T.);
#2550=FACE_OUTER_BOUND('',#3601,.T.);
#2551=FACE_OUTER_BOUND('',#3602,.T.);
#2552=FACE_OUTER_BOUND('',#3603,.T.);
#2553=FACE_OUTER_BOUND('',#3604,.T.);
#2554=FACE_OUTER_BOUND('',#3605,.T.);
#2555=FACE_OUTER_BOUND('',#3606,.T.);
#2556=FACE_OUTER_BOUND('',#3607,.T.);
#2557=FACE_OUTER_BOUND('',#3608,.T.);
#2558=FACE_OUTER_BOUND('',#3609,.T.);
#2559=FACE_OUTER_BOUND('',#3610,.T.);
#2560=FACE_OUTER_BOUND('',#3611,.T.);
#2561=FACE_OUTER_BOUND('',#3612,.T.);
#2562=FACE_OUTER_BOUND('',#3613,.T.);
#2563=FACE_OUTER_BOUND('',#3614,.T.);
#2564=FACE_OUTER_BOUND('',#3615,.T.);
#2565=FACE_OUTER_BOUND('',#3616,.T.);
#2566=FACE_OUTER_BOUND('',#3617,.T.);
#2567=FACE_OUTER_BOUND('',#3618,.T.);
#2568=FACE_OUTER_BOUND('',#3619,.T.);
#2569=FACE_OUTER_BOUND('',#3620,.T.);
#2570=FACE_OUTER_BOUND('',#3621,.T.);
#2571=FACE_OUTER_BOUND('',#3622,.T.);
#2572=FACE_OUTER_BOUND('',#3623,.T.);
#2573=FACE_OUTER_BOUND('',#3624,.T.);
#2574=FACE_OUTER_BOUND('',#3625,.T.);
#2575=FACE_OUTER_BOUND('',#3626,.T.);
#2576=FACE_OUTER_BOUND('',#3627,.T.);
#2577=FACE_OUTER_BOUND('',#3628,.T.);
#2578=FACE_OUTER_BOUND('',#3629,.T.);
#2579=FACE_OUTER_BOUND('',#3630,.T.);
#2580=FACE_OUTER_BOUND('',#3631,.T.);
#2581=FACE_OUTER_BOUND('',#3632,.T.);
#2582=FACE_OUTER_BOUND('',#3633,.T.);
#2583=FACE_OUTER_BOUND('',#3634,.T.);
#2584=FACE_OUTER_BOUND('',#3635,.T.);
#2585=FACE_OUTER_BOUND('',#3636,.T.);
#2586=FACE_OUTER_BOUND('',#3637,.T.);
#2587=FACE_OUTER_BOUND('',#3638,.T.);
#2588=FACE_OUTER_BOUND('',#3639,.T.);
#2589=FACE_OUTER_BOUND('',#3640,.T.);
#2590=FACE_OUTER_BOUND('',#3641,.T.);
#2591=FACE_OUTER_BOUND('',#3642,.T.);
#2592=FACE_OUTER_BOUND('',#3643,.T.);
#2593=FACE_OUTER_BOUND('',#3644,.T.);
#2594=FACE_OUTER_BOUND('',#3645,.T.);
#2595=FACE_OUTER_BOUND('',#3646,.T.);
#2596=FACE_OUTER_BOUND('',#3647,.T.);
#2597=FACE_OUTER_BOUND('',#3648,.T.);
#2598=FACE_OUTER_BOUND('',#3649,.T.);
#2599=FACE_OUTER_BOUND('',#3650,.T.);
#2600=FACE_OUTER_BOUND('',#3651,.T.);
#2601=FACE_OUTER_BOUND('',#3652,.T.);
#2602=FACE_OUTER_BOUND('',#3653,.T.);
#2603=FACE_OUTER_BOUND('',#3654,.T.);
#2604=FACE_OUTER_BOUND('',#3655,.T.);
#2605=FACE_OUTER_BOUND('',#3656,.T.);
#2606=FACE_OUTER_BOUND('',#3657,.T.);
#2607=FACE_OUTER_BOUND('',#3658,.T.);
#2608=FACE_OUTER_BOUND('',#3659,.T.);
#2609=FACE_OUTER_BOUND('',#3660,.T.);
#2610=FACE_OUTER_BOUND('',#3661,.T.);
#2611=FACE_OUTER_BOUND('',#3662,.T.);
#2612=FACE_OUTER_BOUND('',#3663,.T.);
#2613=FACE_OUTER_BOUND('',#3664,.T.);
#2614=FACE_OUTER_BOUND('',#3665,.T.);
#2615=FACE_OUTER_BOUND('',#3666,.T.);
#2616=FACE_OUTER_BOUND('',#3667,.T.);
#2617=FACE_OUTER_BOUND('',#3668,.T.);
#2618=FACE_OUTER_BOUND('',#3669,.T.);
#2619=FACE_OUTER_BOUND('',#3670,.T.);
#2620=FACE_OUTER_BOUND('',#3671,.T.);
#2621=FACE_OUTER_BOUND('',#3672,.T.);
#2622=FACE_OUTER_BOUND('',#3673,.T.);
#2623=FACE_OUTER_BOUND('',#3674,.T.);
#2624=FACE_OUTER_BOUND('',#3675,.T.);
#2625=FACE_OUTER_BOUND('',#3676,.T.);
#2626=FACE_OUTER_BOUND('',#3677,.T.);
#2627=FACE_OUTER_BOUND('',#3678,.T.);
#2628=FACE_OUTER_BOUND('',#3679,.T.);
#2629=FACE_OUTER_BOUND('',#3680,.T.);
#2630=FACE_OUTER_BOUND('',#3681,.T.);
#2631=FACE_OUTER_BOUND('',#3682,.T.);
#2632=FACE_OUTER_BOUND('',#3683,.T.);
#2633=FACE_OUTER_BOUND('',#3684,.T.);
#2634=FACE_OUTER_BOUND('',#3685,.T.);
#2635=FACE_OUTER_BOUND('',#3686,.T.);
#2636=FACE_OUTER_BOUND('',#3687,.T.);
#2637=FACE_OUTER_BOUND('',#3688,.T.);
#2638=FACE_OUTER_BOUND('',#3689,.T.);
#2639=FACE_OUTER_BOUND('',#3690,.T.);
#2640=FACE_OUTER_BOUND('',#3691,.T.);
#2641=FACE_OUTER_BOUND('',#3692,.T.);
#2642=FACE_OUTER_BOUND('',#3693,.T.);
#2643=FACE_OUTER_BOUND('',#3694,.T.);
#2644=FACE_OUTER_BOUND('',#3695,.T.);
#2645=FACE_OUTER_BOUND('',#3696,.T.);
#2646=FACE_OUTER_BOUND('',#3697,.T.);
#2647=EDGE_LOOP('',(#10909,#10910,#10911,#10912));
#2648=EDGE_LOOP('',(#10913,#10914,#10915,#10916));
#2649=EDGE_LOOP('',(#10917,#10918,#10919,#10920,#10921,#10922,#10923,#10924));
#2650=EDGE_LOOP('',(#10925,#10926,#10927,#10928,#10929,#10930,#10931,#10932));
#2651=EDGE_LOOP('',(#10933,#10934,#10935,#10936));
#2652=EDGE_LOOP('',(#10937,#10938,#10939,#10940));
#2653=EDGE_LOOP('',(#10941,#10942,#10943,#10944));
#2654=EDGE_LOOP('',(#10945,#10946,#10947,#10948));
#2655=EDGE_LOOP('',(#10949,#10950,#10951,#10952));
#2656=EDGE_LOOP('',(#10953,#10954,#10955,#10956));
#2657=EDGE_LOOP('',(#10957,#10958,#10959,#10960));
#2658=EDGE_LOOP('',(#10961,#10962,#10963,#10964));
#2659=EDGE_LOOP('',(#10965,#10966,#10967,#10968));
#2660=EDGE_LOOP('',(#10969,#10970,#10971,#10972,#10973,#10974,#10975,#10976));
#2661=EDGE_LOOP('',(#10977,#10978,#10979,#10980,#10981,#10982,#10983,#10984));
#2662=EDGE_LOOP('',(#10985,#10986,#10987,#10988));
#2663=EDGE_LOOP('',(#10989,#10990,#10991,#10992));
#2664=EDGE_LOOP('',(#10993,#10994,#10995,#10996));
#2665=EDGE_LOOP('',(#10997,#10998,#10999,#11000));
#2666=EDGE_LOOP('',(#11001,#11002,#11003,#11004));
#2667=EDGE_LOOP('',(#11005,#11006,#11007,#11008));
#2668=EDGE_LOOP('',(#11009,#11010,#11011,#11012,#11013,#11014,#11015,#11016));
#2669=EDGE_LOOP('',(#11017,#11018,#11019,#11020,#11021,#11022,#11023,#11024));
#2670=EDGE_LOOP('',(#11025,#11026,#11027,#11028));
#2671=EDGE_LOOP('',(#11029,#11030,#11031,#11032));
#2672=EDGE_LOOP('',(#11033,#11034,#11035,#11036));
#2673=EDGE_LOOP('',(#11037,#11038,#11039,#11040));
#2674=EDGE_LOOP('',(#11041,#11042,#11043,#11044));
#2675=EDGE_LOOP('',(#11045,#11046,#11047,#11048));
#2676=EDGE_LOOP('',(#11049,#11050,#11051,#11052));
#2677=EDGE_LOOP('',(#11053,#11054,#11055,#11056));
#2678=EDGE_LOOP('',(#11057,#11058,#11059,#11060,#11061,#11062,#11063,#11064));
#2679=EDGE_LOOP('',(#11065,#11066,#11067,#11068,#11069,#11070,#11071,#11072));
#2680=EDGE_LOOP('',(#11073,#11074,#11075,#11076));
#2681=EDGE_LOOP('',(#11077,#11078,#11079,#11080));
#2682=EDGE_LOOP('',(#11081,#11082,#11083,#11084));
#2683=EDGE_LOOP('',(#11085,#11086,#11087,#11088));
#2684=EDGE_LOOP('',(#11089,#11090,#11091,#11092));
#2685=EDGE_LOOP('',(#11093,#11094,#11095,#11096));
#2686=EDGE_LOOP('',(#11097,#11098,#11099,#11100));
#2687=EDGE_LOOP('',(#11101,#11102,#11103,#11104));
#2688=EDGE_LOOP('',(#11105,#11106));
#2689=EDGE_LOOP('',(#11107,#11108,#11109,#11110,#11111,#11112,#11113,#11114));
#2690=EDGE_LOOP('',(#11115,#11116));
#2691=EDGE_LOOP('',(#11117,#11118,#11119,#11120));
#2692=EDGE_LOOP('',(#11121,#11122,#11123,#11124));
#2693=EDGE_LOOP('',(#11125,#11126,#11127,#11128));
#2694=EDGE_LOOP('',(#11129,#11130,#11131,#11132));
#2695=EDGE_LOOP('',(#11133,#11134));
#2696=EDGE_LOOP('',(#11135,#11136,#11137,#11138,#11139,#11140,#11141,#11142));
#2697=EDGE_LOOP('',(#11143,#11144));
#2698=EDGE_LOOP('',(#11145,#11146,#11147,#11148));
#2699=EDGE_LOOP('',(#11149,#11150,#11151,#11152));
#2700=EDGE_LOOP('',(#11153,#11154,#11155,#11156,#11157,#11158,#11159,#11160));
#2701=EDGE_LOOP('',(#11161,#11162,#11163,#11164));
#2702=EDGE_LOOP('',(#11165,#11166,#11167,#11168,#11169,#11170,#11171,#11172));
#2703=EDGE_LOOP('',(#11173,#11174,#11175,#11176));
#2704=EDGE_LOOP('',(#11177,#11178,#11179,#11180));
#2705=EDGE_LOOP('',(#11181,#11182,#11183,#11184));
#2706=EDGE_LOOP('',(#11185,#11186,#11187,#11188));
#2707=EDGE_LOOP('',(#11189,#11190,#11191,#11192));
#2708=EDGE_LOOP('',(#11193,#11194,#11195,#11196));
#2709=EDGE_LOOP('',(#11197,#11198,#11199));
#2710=EDGE_LOOP('',(#11200,#11201,#11202,#11203));
#2711=EDGE_LOOP('',(#11204,#11205,#11206,#11207));
#2712=EDGE_LOOP('',(#11208,#11209,#11210,#11211,#11212));
#2713=EDGE_LOOP('',(#11213,#11214,#11215,#11216));
#2714=EDGE_LOOP('',(#11217));
#2715=EDGE_LOOP('',(#11218,#11219,#11220,#11221,#11222));
#2716=EDGE_LOOP('',(#11223));
#2717=EDGE_LOOP('',(#11224));
#2718=EDGE_LOOP('',(#11225));
#2719=EDGE_LOOP('',(#11226));
#2720=EDGE_LOOP('',(#11227,#11228,#11229,#11230));
#2721=EDGE_LOOP('',(#11231,#11232,#11233,#11234));
#2722=EDGE_LOOP('',(#11235,#11236,#11237,#11238));
#2723=EDGE_LOOP('',(#11239,#11240,#11241,#11242));
#2724=EDGE_LOOP('',(#11243,#11244,#11245,#11246));
#2725=EDGE_LOOP('',(#11247,#11248,#11249,#11250));
#2726=EDGE_LOOP('',(#11251,#11252,#11253,#11254));
#2727=EDGE_LOOP('',(#11255,#11256,#11257,#11258));
#2728=EDGE_LOOP('',(#11259,#11260,#11261,#11262));
#2729=EDGE_LOOP('',(#11263,#11264,#11265,#11266));
#2730=EDGE_LOOP('',(#11267,#11268,#11269,#11270));
#2731=EDGE_LOOP('',(#11271,#11272,#11273,#11274));
#2732=EDGE_LOOP('',(#11275,#11276,#11277,#11278));
#2733=EDGE_LOOP('',(#11279,#11280,#11281,#11282));
#2734=EDGE_LOOP('',(#11283,#11284,#11285,#11286));
#2735=EDGE_LOOP('',(#11287,#11288,#11289,#11290));
#2736=EDGE_LOOP('',(#11291,#11292,#11293,#11294));
#2737=EDGE_LOOP('',(#11295,#11296,#11297,#11298));
#2738=EDGE_LOOP('',(#11299,#11300,#11301,#11302));
#2739=EDGE_LOOP('',(#11303,#11304,#11305,#11306));
#2740=EDGE_LOOP('',(#11307,#11308,#11309,#11310));
#2741=EDGE_LOOP('',(#11311,#11312,#11313,#11314));
#2742=EDGE_LOOP('',(#11315,#11316,#11317,#11318));
#2743=EDGE_LOOP('',(#11319,#11320,#11321,#11322));
#2744=EDGE_LOOP('',(#11323,#11324,#11325,#11326));
#2745=EDGE_LOOP('',(#11327,#11328,#11329));
#2746=EDGE_LOOP('',(#11330,#11331,#11332,#11333,#11334,#11335));
#2747=EDGE_LOOP('',(#11336,#11337,#11338,#11339));
#2748=EDGE_LOOP('',(#11340,#11341,#11342,#11343));
#2749=EDGE_LOOP('',(#11344,#11345,#11346,#11347));
#2750=EDGE_LOOP('',(#11348,#11349,#11350,#11351));
#2751=EDGE_LOOP('',(#11352,#11353,#11354,#11355));
#2752=EDGE_LOOP('',(#11356,#11357,#11358,#11359));
#2753=EDGE_LOOP('',(#11360,#11361,#11362,#11363));
#2754=EDGE_LOOP('',(#11364,#11365,#11366,#11367));
#2755=EDGE_LOOP('',(#11368,#11369,#11370,#11371));
#2756=EDGE_LOOP('',(#11372,#11373,#11374,#11375));
#2757=EDGE_LOOP('',(#11376,#11377,#11378,#11379));
#2758=EDGE_LOOP('',(#11380,#11381,#11382,#11383));
#2759=EDGE_LOOP('',(#11384,#11385,#11386,#11387));
#2760=EDGE_LOOP('',(#11388,#11389,#11390,#11391));
#2761=EDGE_LOOP('',(#11392,#11393,#11394,#11395));
#2762=EDGE_LOOP('',(#11396,#11397,#11398,#11399));
#2763=EDGE_LOOP('',(#11400,#11401,#11402,#11403));
#2764=EDGE_LOOP('',(#11404,#11405,#11406,#11407));
#2765=EDGE_LOOP('',(#11408,#11409,#11410,#11411));
#2766=EDGE_LOOP('',(#11412,#11413,#11414,#11415));
#2767=EDGE_LOOP('',(#11416,#11417,#11418,#11419));
#2768=EDGE_LOOP('',(#11420,#11421,#11422,#11423));
#2769=EDGE_LOOP('',(#11424,#11425,#11426,#11427));
#2770=EDGE_LOOP('',(#11428,#11429,#11430,#11431,#11432));
#2771=EDGE_LOOP('',(#11433,#11434,#11435,#11436,#11437,#11438,#11439,#11440,
#11441,#11442,#11443,#11444));
#2772=EDGE_LOOP('',(#11445,#11446,#11447,#11448));
#2773=EDGE_LOOP('',(#11449,#11450,#11451,#11452,#11453,#11454,#11455,#11456,
#11457,#11458,#11459,#11460));
#2774=EDGE_LOOP('',(#11461,#11462,#11463,#11464));
#2775=EDGE_LOOP('',(#11465,#11466,#11467,#11468));
#2776=EDGE_LOOP('',(#11469,#11470,#11471,#11472));
#2777=EDGE_LOOP('',(#11473,#11474,#11475,#11476));
#2778=EDGE_LOOP('',(#11477));
#2779=EDGE_LOOP('',(#11478,#11479,#11480,#11481));
#2780=EDGE_LOOP('',(#11482));
#2781=EDGE_LOOP('',(#11483));
#2782=EDGE_LOOP('',(#11484));
#2783=EDGE_LOOP('',(#11485));
#2784=EDGE_LOOP('',(#11486));
#2785=EDGE_LOOP('',(#11487));
#2786=EDGE_LOOP('',(#11488));
#2787=EDGE_LOOP('',(#11489));
#2788=EDGE_LOOP('',(#11490,#11491,#11492,#11493));
#2789=EDGE_LOOP('',(#11494,#11495,#11496,#11497,#11498,#11499));
#2790=EDGE_LOOP('',(#11500,#11501,#11502,#11503));
#2791=EDGE_LOOP('',(#11504,#11505,#11506,#11507,#11508,#11509));
#2792=EDGE_LOOP('',(#11510,#11511,#11512,#11513));
#2793=EDGE_LOOP('',(#11514,#11515,#11516,#11517));
#2794=EDGE_LOOP('',(#11518,#11519,#11520,#11521,#11522,#11523,#11524,#11525,
#11526,#11527,#11528,#11529,#11530,#11531,#11532,#11533,#11534,#11535,#11536,
#11537,#11538,#11539,#11540,#11541,#11542,#11543,#11544,#11545,#11546,#11547,
#11548,#11549,#11550,#11551,#11552,#11553,#11554,#11555,#11556,#11557,#11558,
#11559,#11560,#11561,#11562,#11563,#11564,#11565,#11566,#11567,#11568,#11569,
#11570,#11571));
#2795=EDGE_LOOP('',(#11572,#11573,#11574,#11575,#11576,#11577,#11578,#11579,
#11580,#11581,#11582,#11583,#11584,#11585,#11586,#11587,#11588,#11589,#11590,
#11591,#11592,#11593,#11594,#11595,#11596,#11597,#11598,#11599,#11600,#11601,
#11602,#11603,#11604,#11605,#11606,#11607,#11608,#11609,#11610,#11611,#11612,
#11613,#11614,#11615,#11616,#11617,#11618,#11619,#11620,#11621,#11622,#11623,
#11624));
#2796=EDGE_LOOP('',(#11625,#11626,#11627,#11628));
#2797=EDGE_LOOP('',(#11629,#11630,#11631,#11632));
#2798=EDGE_LOOP('',(#11633));
#2799=EDGE_LOOP('',(#11634));
#2800=EDGE_LOOP('',(#11635));
#2801=EDGE_LOOP('',(#11636));
#2802=EDGE_LOOP('',(#11637,#11638,#11639,#11640));
#2803=EDGE_LOOP('',(#11641,#11642,#11643,#11644));
#2804=EDGE_LOOP('',(#11645));
#2805=EDGE_LOOP('',(#11646));
#2806=EDGE_LOOP('',(#11647));
#2807=EDGE_LOOP('',(#11648));
#2808=EDGE_LOOP('',(#11649,#11650,#11651,#11652,#11653));
#2809=EDGE_LOOP('',(#11654,#11655,#11656,#11657));
#2810=EDGE_LOOP('',(#11658,#11659,#11660,#11661));
#2811=EDGE_LOOP('',(#11662,#11663,#11664,#11665,#11666));
#2812=EDGE_LOOP('',(#11667));
#2813=EDGE_LOOP('',(#11668));
#2814=EDGE_LOOP('',(#11669,#11670,#11671,#11672));
#2815=EDGE_LOOP('',(#11673,#11674,#11675,#11676));
#2816=EDGE_LOOP('',(#11677,#11678,#11679,#11680));
#2817=EDGE_LOOP('',(#11681,#11682,#11683,#11684));
#2818=EDGE_LOOP('',(#11685,#11686,#11687,#11688));
#2819=EDGE_LOOP('',(#11689,#11690));
#2820=EDGE_LOOP('',(#11691));
#2821=EDGE_LOOP('',(#11692,#11693,#11694,#11695));
#2822=EDGE_LOOP('',(#11696));
#2823=EDGE_LOOP('',(#11697));
#2824=EDGE_LOOP('',(#11698));
#2825=EDGE_LOOP('',(#11699));
#2826=EDGE_LOOP('',(#11700));
#2827=EDGE_LOOP('',(#11701,#11702,#11703,#11704));
#2828=EDGE_LOOP('',(#11705,#11706,#11707));
#2829=EDGE_LOOP('',(#11708,#11709,#11710,#11711));
#2830=EDGE_LOOP('',(#11712,#11713,#11714,#11715,#11716,#11717));
#2831=EDGE_LOOP('',(#11718,#11719,#11720,#11721));
#2832=EDGE_LOOP('',(#11722,#11723,#11724,#11725,#11726,#11727,#11728,#11729,
#11730));
#2833=EDGE_LOOP('',(#11731,#11732,#11733,#11734,#11735,#11736,#11737,#11738,
#11739));
#2834=EDGE_LOOP('',(#11740,#11741,#11742,#11743,#11744,#11745,#11746));
#2835=EDGE_LOOP('',(#11747,#11748,#11749,#11750,#11751,#11752,#11753,#11754));
#2836=EDGE_LOOP('',(#11755));
#2837=EDGE_LOOP('',(#11756));
#2838=EDGE_LOOP('',(#11757,#11758,#11759));
#2839=EDGE_LOOP('',(#11760,#11761,#11762));
#2840=EDGE_LOOP('',(#11763,#11764,#11765,#11766,#11767,#11768,#11769,#11770,
#11771,#11772,#11773,#11774,#11775,#11776,#11777));
#2841=EDGE_LOOP('',(#11778,#11779,#11780,#11781));
#2842=EDGE_LOOP('',(#11782,#11783,#11784,#11785));
#2843=EDGE_LOOP('',(#11786,#11787,#11788));
#2844=EDGE_LOOP('',(#11789,#11790,#11791));
#2845=EDGE_LOOP('',(#11792,#11793,#11794));
#2846=EDGE_LOOP('',(#11795,#11796,#11797,#11798));
#2847=EDGE_LOOP('',(#11799,#11800,#11801,#11802));
#2848=EDGE_LOOP('',(#11803,#11804,#11805));
#2849=EDGE_LOOP('',(#11806,#11807,#11808,#11809));
#2850=EDGE_LOOP('',(#11810,#11811,#11812));
#2851=EDGE_LOOP('',(#11813,#11814,#11815,#11816));
#2852=EDGE_LOOP('',(#11817,#11818,#11819));
#2853=EDGE_LOOP('',(#11820,#11821,#11822,#11823,#11824));
#2854=EDGE_LOOP('',(#11825,#11826,#11827,#11828,#11829));
#2855=EDGE_LOOP('',(#11830,#11831,#11832,#11833,#11834));
#2856=EDGE_LOOP('',(#11835,#11836,#11837));
#2857=EDGE_LOOP('',(#11838,#11839,#11840,#11841));
#2858=EDGE_LOOP('',(#11842,#11843,#11844,#11845));
#2859=EDGE_LOOP('',(#11846,#11847,#11848));
#2860=EDGE_LOOP('',(#11849,#11850,#11851,#11852));
#2861=EDGE_LOOP('',(#11853,#11854,#11855,#11856));
#2862=EDGE_LOOP('',(#11857,#11858,#11859,#11860));
#2863=EDGE_LOOP('',(#11861,#11862,#11863,#11864));
#2864=EDGE_LOOP('',(#11865,#11866,#11867,#11868));
#2865=EDGE_LOOP('',(#11869,#11870,#11871,#11872));
#2866=EDGE_LOOP('',(#11873,#11874,#11875,#11876,#11877));
#2867=EDGE_LOOP('',(#11878,#11879,#11880,#11881));
#2868=EDGE_LOOP('',(#11882,#11883,#11884,#11885));
#2869=EDGE_LOOP('',(#11886));
#2870=EDGE_LOOP('',(#11887,#11888));
#2871=EDGE_LOOP('',(#11889));
#2872=EDGE_LOOP('',(#11890,#11891));
#2873=EDGE_LOOP('',(#11892));
#2874=EDGE_LOOP('',(#11893,#11894,#11895,#11896,#11897,#11898,#11899));
#2875=EDGE_LOOP('',(#11900,#11901,#11902,#11903,#11904,#11905,#11906,#11907));
#2876=EDGE_LOOP('',(#11908,#11909,#11910,#11911));
#2877=EDGE_LOOP('',(#11912,#11913,#11914,#11915,#11916,#11917));
#2878=EDGE_LOOP('',(#11918,#11919,#11920,#11921,#11922,#11923));
#2879=EDGE_LOOP('',(#11924,#11925,#11926,#11927,#11928));
#2880=EDGE_LOOP('',(#11929,#11930,#11931,#11932,#11933,#11934,#11935,#11936));
#2881=EDGE_LOOP('',(#11937,#11938,#11939,#11940,#11941,#11942,#11943,#11944,
#11945,#11946,#11947,#11948,#11949));
#2882=EDGE_LOOP('',(#11950));
#2883=EDGE_LOOP('',(#11951));
#2884=EDGE_LOOP('',(#11952,#11953,#11954,#11955,#11956));
#2885=EDGE_LOOP('',(#11957,#11958,#11959,#11960,#11961));
#2886=EDGE_LOOP('',(#11962,#11963,#11964,#11965));
#2887=EDGE_LOOP('',(#11966,#11967,#11968,#11969));
#2888=EDGE_LOOP('',(#11970,#11971,#11972,#11973));
#2889=EDGE_LOOP('',(#11974,#11975,#11976,#11977));
#2890=EDGE_LOOP('',(#11978,#11979,#11980,#11981,#11982,#11983,#11984));
#2891=EDGE_LOOP('',(#11985,#11986,#11987,#11988));
#2892=EDGE_LOOP('',(#11989,#11990,#11991,#11992));
#2893=EDGE_LOOP('',(#11993,#11994,#11995,#11996));
#2894=EDGE_LOOP('',(#11997,#11998,#11999,#12000));
#2895=EDGE_LOOP('',(#12001,#12002,#12003,#12004));
#2896=EDGE_LOOP('',(#12005,#12006,#12007,#12008));
#2897=EDGE_LOOP('',(#12009,#12010,#12011,#12012,#12013));
#2898=EDGE_LOOP('',(#12014,#12015,#12016,#12017));
#2899=EDGE_LOOP('',(#12018,#12019,#12020,#12021));
#2900=EDGE_LOOP('',(#12022));
#2901=EDGE_LOOP('',(#12023,#12024));
#2902=EDGE_LOOP('',(#12025));
#2903=EDGE_LOOP('',(#12026,#12027));
#2904=EDGE_LOOP('',(#12028));
#2905=EDGE_LOOP('',(#12029,#12030,#12031,#12032,#12033));
#2906=EDGE_LOOP('',(#12034,#12035,#12036,#12037));
#2907=EDGE_LOOP('',(#12038,#12039,#12040,#12041,#12042));
#2908=EDGE_LOOP('',(#12043,#12044,#12045,#12046,#12047,#12048));
#2909=EDGE_LOOP('',(#12049,#12050,#12051,#12052,#12053));
#2910=EDGE_LOOP('',(#12054,#12055,#12056,#12057));
#2911=EDGE_LOOP('',(#12058,#12059,#12060,#12061,#12062));
#2912=EDGE_LOOP('',(#12063));
#2913=EDGE_LOOP('',(#12064));
#2914=EDGE_LOOP('',(#12065));
#2915=EDGE_LOOP('',(#12066));
#2916=EDGE_LOOP('',(#12067));
#2917=EDGE_LOOP('',(#12068));
#2918=EDGE_LOOP('',(#12069,#12070,#12071,#12072));
#2919=EDGE_LOOP('',(#12073,#12074,#12075,#12076));
#2920=EDGE_LOOP('',(#12077,#12078,#12079,#12080));
#2921=EDGE_LOOP('',(#12081,#12082,#12083,#12084));
#2922=EDGE_LOOP('',(#12085,#12086,#12087,#12088));
#2923=EDGE_LOOP('',(#12089,#12090,#12091,#12092));
#2924=EDGE_LOOP('',(#12093,#12094,#12095,#12096));
#2925=EDGE_LOOP('',(#12097,#12098,#12099,#12100));
#2926=EDGE_LOOP('',(#12101,#12102,#12103,#12104));
#2927=EDGE_LOOP('',(#12105,#12106,#12107,#12108));
#2928=EDGE_LOOP('',(#12109,#12110,#12111,#12112));
#2929=EDGE_LOOP('',(#12113,#12114,#12115,#12116));
#2930=EDGE_LOOP('',(#12117,#12118,#12119,#12120));
#2931=EDGE_LOOP('',(#12121,#12122,#12123,#12124));
#2932=EDGE_LOOP('',(#12125,#12126,#12127,#12128));
#2933=EDGE_LOOP('',(#12129,#12130,#12131,#12132));
#2934=EDGE_LOOP('',(#12133,#12134,#12135,#12136));
#2935=EDGE_LOOP('',(#12137,#12138,#12139,#12140));
#2936=EDGE_LOOP('',(#12141,#12142,#12143,#12144));
#2937=EDGE_LOOP('',(#12145,#12146,#12147,#12148));
#2938=EDGE_LOOP('',(#12149,#12150,#12151,#12152));
#2939=EDGE_LOOP('',(#12153,#12154,#12155,#12156));
#2940=EDGE_LOOP('',(#12157,#12158,#12159,#12160));
#2941=EDGE_LOOP('',(#12161,#12162,#12163,#12164));
#2942=EDGE_LOOP('',(#12165,#12166,#12167,#12168));
#2943=EDGE_LOOP('',(#12169,#12170,#12171,#12172));
#2944=EDGE_LOOP('',(#12173,#12174,#12175,#12176));
#2945=EDGE_LOOP('',(#12177,#12178,#12179,#12180));
#2946=EDGE_LOOP('',(#12181,#12182,#12183,#12184));
#2947=EDGE_LOOP('',(#12185,#12186,#12187,#12188));
#2948=EDGE_LOOP('',(#12189,#12190,#12191,#12192,#12193,#12194,#12195,#12196,
#12197,#12198,#12199,#12200));
#2949=EDGE_LOOP('',(#12201,#12202,#12203,#12204));
#2950=EDGE_LOOP('',(#12205,#12206,#12207,#12208,#12209,#12210,#12211,#12212,
#12213,#12214,#12215,#12216));
#2951=EDGE_LOOP('',(#12217));
#2952=EDGE_LOOP('',(#12218));
#2953=EDGE_LOOP('',(#12219));
#2954=EDGE_LOOP('',(#12220));
#2955=EDGE_LOOP('',(#12221,#12222,#12223,#12224));
#2956=EDGE_LOOP('',(#12225,#12226,#12227,#12228));
#2957=EDGE_LOOP('',(#12229,#12230,#12231,#12232));
#2958=EDGE_LOOP('',(#12233,#12234,#12235,#12236));
#2959=EDGE_LOOP('',(#12237,#12238,#12239,#12240));
#2960=EDGE_LOOP('',(#12241,#12242,#12243));
#2961=EDGE_LOOP('',(#12244,#12245,#12246));
#2962=EDGE_LOOP('',(#12247,#12248,#12249,#12250));
#2963=EDGE_LOOP('',(#12251,#12252,#12253));
#2964=EDGE_LOOP('',(#12254,#12255,#12256));
#2965=EDGE_LOOP('',(#12257,#12258,#12259,#12260));
#2966=EDGE_LOOP('',(#12261,#12262,#12263,#12264));
#2967=EDGE_LOOP('',(#12265,#12266,#12267));
#2968=EDGE_LOOP('',(#12268,#12269,#12270));
#2969=EDGE_LOOP('',(#12271,#12272,#12273,#12274));
#2970=EDGE_LOOP('',(#12275,#12276,#12277));
#2971=EDGE_LOOP('',(#12278,#12279,#12280));
#2972=EDGE_LOOP('',(#12281,#12282,#12283,#12284));
#2973=EDGE_LOOP('',(#12285,#12286,#12287));
#2974=EDGE_LOOP('',(#12288,#12289,#12290));
#2975=EDGE_LOOP('',(#12291,#12292,#12293,#12294));
#2976=EDGE_LOOP('',(#12295,#12296,#12297));
#2977=EDGE_LOOP('',(#12298,#12299,#12300));
#2978=EDGE_LOOP('',(#12301,#12302,#12303,#12304));
#2979=EDGE_LOOP('',(#12305,#12306,#12307));
#2980=EDGE_LOOP('',(#12308,#12309,#12310));
#2981=EDGE_LOOP('',(#12311,#12312,#12313,#12314));
#2982=EDGE_LOOP('',(#12315,#12316,#12317,#12318));
#2983=EDGE_LOOP('',(#12319,#12320,#12321));
#2984=EDGE_LOOP('',(#12322,#12323,#12324));
#2985=EDGE_LOOP('',(#12325,#12326,#12327));
#2986=EDGE_LOOP('',(#12328,#12329,#12330));
#2987=EDGE_LOOP('',(#12331,#12332,#12333,#12334));
#2988=EDGE_LOOP('',(#12335,#12336,#12337));
#2989=EDGE_LOOP('',(#12338,#12339,#12340));
#2990=EDGE_LOOP('',(#12341,#12342,#12343,#12344));
#2991=EDGE_LOOP('',(#12345,#12346,#12347));
#2992=EDGE_LOOP('',(#12348,#12349,#12350));
#2993=EDGE_LOOP('',(#12351,#12352,#12353,#12354));
#2994=EDGE_LOOP('',(#12355,#12356,#12357,#12358));
#2995=EDGE_LOOP('',(#12359,#12360,#12361));
#2996=EDGE_LOOP('',(#12362,#12363,#12364));
#2997=EDGE_LOOP('',(#12365,#12366,#12367,#12368));
#2998=EDGE_LOOP('',(#12369,#12370,#12371,#12372));
#2999=EDGE_LOOP('',(#12373,#12374,#12375,#12376,#12377));
#3000=EDGE_LOOP('',(#12378,#12379,#12380,#12381,#12382));
#3001=EDGE_LOOP('',(#12383,#12384,#12385,#12386));
#3002=EDGE_LOOP('',(#12387,#12388,#12389,#12390));
#3003=EDGE_LOOP('',(#12391,#12392,#12393,#12394,#12395));
#3004=EDGE_LOOP('',(#12396,#12397,#12398,#12399,#12400));
#3005=EDGE_LOOP('',(#12401,#12402,#12403,#12404));
#3006=EDGE_LOOP('',(#12405,#12406,#12407,#12408));
#3007=EDGE_LOOP('',(#12409,#12410,#12411,#12412));
#3008=EDGE_LOOP('',(#12413,#12414,#12415,#12416,#12417,#12418,#12419));
#3009=EDGE_LOOP('',(#12420,#12421,#12422,#12423));
#3010=EDGE_LOOP('',(#12424,#12425,#12426,#12427,#12428));
#3011=EDGE_LOOP('',(#12429,#12430,#12431,#12432,#12433,#12434));
#3012=EDGE_LOOP('',(#12435,#12436,#12437,#12438,#12439));
#3013=EDGE_LOOP('',(#12440,#12441,#12442,#12443,#12444));
#3014=EDGE_LOOP('',(#12445,#12446,#12447,#12448));
#3015=EDGE_LOOP('',(#12449,#12450,#12451,#12452));
#3016=EDGE_LOOP('',(#12453,#12454,#12455,#12456,#12457,#12458,#12459,#12460,
#12461,#12462,#12463,#12464,#12465,#12466,#12467,#12468));
#3017=EDGE_LOOP('',(#12469));
#3018=EDGE_LOOP('',(#12470));
#3019=EDGE_LOOP('',(#12471,#12472,#12473,#12474));
#3020=EDGE_LOOP('',(#12475,#12476,#12477,#12478,#12479,#12480,#12481,#12482,
#12483,#12484,#12485,#12486,#12487,#12488,#12489,#12490,#12491,#12492,#12493,
#12494));
#3021=EDGE_LOOP('',(#12495,#12496,#12497,#12498));
#3022=EDGE_LOOP('',(#12499,#12500,#12501,#12502,#12503,#12504,#12505,#12506));
#3023=EDGE_LOOP('',(#12507));
#3024=EDGE_LOOP('',(#12508));
#3025=EDGE_LOOP('',(#12509,#12510,#12511,#12512,#12513,#12514,#12515));
#3026=EDGE_LOOP('',(#12516));
#3027=EDGE_LOOP('',(#12517,#12518,#12519,#12520,#12521,#12522,#12523,#12524,
#12525));
#3028=EDGE_LOOP('',(#12526));
#3029=EDGE_LOOP('',(#12527,#12528,#12529,#12530));
#3030=EDGE_LOOP('',(#12531,#12532,#12533,#12534,#12535,#12536,#12537,#12538,
#12539,#12540,#12541));
#3031=EDGE_LOOP('',(#12542,#12543,#12544,#12545,#12546,#12547,#12548,#12549));
#3032=EDGE_LOOP('',(#12550));
#3033=EDGE_LOOP('',(#12551,#12552,#12553,#12554));
#3034=EDGE_LOOP('',(#12555,#12556,#12557,#12558,#12559,#12560));
#3035=EDGE_LOOP('',(#12561,#12562,#12563,#12564));
#3036=EDGE_LOOP('',(#12565,#12566,#12567,#12568));
#3037=EDGE_LOOP('',(#12569,#12570,#12571,#12572));
#3038=EDGE_LOOP('',(#12573,#12574,#12575,#12576));
#3039=EDGE_LOOP('',(#12577,#12578,#12579,#12580,#12581,#12582));
#3040=EDGE_LOOP('',(#12583,#12584,#12585,#12586,#12587,#12588,#12589));
#3041=EDGE_LOOP('',(#12590));
#3042=EDGE_LOOP('',(#12591,#12592,#12593,#12594));
#3043=EDGE_LOOP('',(#12595,#12596,#12597,#12598));
#3044=EDGE_LOOP('',(#12599,#12600,#12601,#12602));
#3045=EDGE_LOOP('',(#12603,#12604,#12605,#12606));
#3046=EDGE_LOOP('',(#12607,#12608,#12609,#12610,#12611));
#3047=EDGE_LOOP('',(#12612));
#3048=EDGE_LOOP('',(#12613,#12614,#12615,#12616));
#3049=EDGE_LOOP('',(#12617,#12618,#12619,#12620));
#3050=EDGE_LOOP('',(#12621,#12622,#12623,#12624));
#3051=EDGE_LOOP('',(#12625,#12626,#12627,#12628));
#3052=EDGE_LOOP('',(#12629,#12630,#12631,#12632));
#3053=EDGE_LOOP('',(#12633,#12634,#12635,#12636));
#3054=EDGE_LOOP('',(#12637,#12638,#12639,#12640));
#3055=EDGE_LOOP('',(#12641,#12642,#12643,#12644));
#3056=EDGE_LOOP('',(#12645,#12646,#12647));
#3057=EDGE_LOOP('',(#12648,#12649,#12650,#12651));
#3058=EDGE_LOOP('',(#12652,#12653,#12654,#12655));
#3059=EDGE_LOOP('',(#12656,#12657,#12658,#12659));
#3060=EDGE_LOOP('',(#12660,#12661,#12662,#12663));
#3061=EDGE_LOOP('',(#12664,#12665,#12666,#12667));
#3062=EDGE_LOOP('',(#12668,#12669,#12670,#12671));
#3063=EDGE_LOOP('',(#12672,#12673,#12674,#12675));
#3064=EDGE_LOOP('',(#12676,#12677,#12678));
#3065=EDGE_LOOP('',(#12679,#12680,#12681));
#3066=EDGE_LOOP('',(#12682,#12683,#12684,#12685));
#3067=EDGE_LOOP('',(#12686,#12687,#12688,#12689));
#3068=EDGE_LOOP('',(#12690,#12691,#12692,#12693));
#3069=EDGE_LOOP('',(#12694,#12695,#12696,#12697));
#3070=EDGE_LOOP('',(#12698,#12699,#12700));
#3071=EDGE_LOOP('',(#12701,#12702,#12703,#12704));
#3072=EDGE_LOOP('',(#12705,#12706,#12707));
#3073=EDGE_LOOP('',(#12708,#12709,#12710,#12711));
#3074=EDGE_LOOP('',(#12712,#12713,#12714,#12715));
#3075=EDGE_LOOP('',(#12716,#12717,#12718,#12719));
#3076=EDGE_LOOP('',(#12720,#12721,#12722,#12723));
#3077=EDGE_LOOP('',(#12724,#12725,#12726,#12727));
#3078=EDGE_LOOP('',(#12728,#12729,#12730));
#3079=EDGE_LOOP('',(#12731,#12732,#12733,#12734));
#3080=EDGE_LOOP('',(#12735,#12736,#12737,#12738));
#3081=EDGE_LOOP('',(#12739,#12740,#12741,#12742));
#3082=EDGE_LOOP('',(#12743,#12744,#12745,#12746));
#3083=EDGE_LOOP('',(#12747,#12748,#12749,#12750,#12751));
#3084=EDGE_LOOP('',(#12752,#12753,#12754,#12755,#12756));
#3085=EDGE_LOOP('',(#12757,#12758,#12759,#12760,#12761,#12762));
#3086=EDGE_LOOP('',(#12763));
#3087=EDGE_LOOP('',(#12764));
#3088=EDGE_LOOP('',(#12765,#12766,#12767,#12768));
#3089=EDGE_LOOP('',(#12769,#12770,#12771,#12772,#12773,#12774));
#3090=EDGE_LOOP('',(#12775,#12776,#12777,#12778));
#3091=EDGE_LOOP('',(#12779,#12780,#12781,#12782));
#3092=EDGE_LOOP('',(#12783,#12784,#12785,#12786));
#3093=EDGE_LOOP('',(#12787,#12788,#12789,#12790));
#3094=EDGE_LOOP('',(#12791,#12792,#12793,#12794));
#3095=EDGE_LOOP('',(#12795,#12796,#12797,#12798));
#3096=EDGE_LOOP('',(#12799,#12800,#12801,#12802));
#3097=EDGE_LOOP('',(#12803,#12804,#12805,#12806,#12807));
#3098=EDGE_LOOP('',(#12808));
#3099=EDGE_LOOP('',(#12809,#12810,#12811,#12812,#12813));
#3100=EDGE_LOOP('',(#12814));
#3101=EDGE_LOOP('',(#12815,#12816,#12817,#12818,#12819));
#3102=EDGE_LOOP('',(#12820,#12821,#12822,#12823,#12824,#12825,#12826,#12827,
#12828));
#3103=EDGE_LOOP('',(#12829));
#3104=EDGE_LOOP('',(#12830,#12831,#12832,#12833));
#3105=EDGE_LOOP('',(#12834,#12835,#12836,#12837));
#3106=EDGE_LOOP('',(#12838,#12839,#12840,#12841,#12842,#12843,#12844,#12845,
#12846));
#3107=EDGE_LOOP('',(#12847));
#3108=EDGE_LOOP('',(#12848,#12849,#12850,#12851,#12852));
#3109=EDGE_LOOP('',(#12853));
#3110=EDGE_LOOP('',(#12854,#12855,#12856,#12857,#12858));
#3111=EDGE_LOOP('',(#12859));
#3112=EDGE_LOOP('',(#12860,#12861,#12862,#12863));
#3113=EDGE_LOOP('',(#12864));
#3114=EDGE_LOOP('',(#12865));
#3115=EDGE_LOOP('',(#12866));
#3116=EDGE_LOOP('',(#12867));
#3117=EDGE_LOOP('',(#12868));
#3118=EDGE_LOOP('',(#12869,#12870,#12871,#12872));
#3119=EDGE_LOOP('',(#12873,#12874));
#3120=EDGE_LOOP('',(#12875));
#3121=EDGE_LOOP('',(#12876));
#3122=EDGE_LOOP('',(#12877,#12878,#12879,#12880));
#3123=EDGE_LOOP('',(#12881,#12882,#12883,#12884,#12885));
#3124=EDGE_LOOP('',(#12886,#12887,#12888,#12889,#12890,#12891));
#3125=EDGE_LOOP('',(#12892,#12893,#12894,#12895,#12896,#12897));
#3126=EDGE_LOOP('',(#12898,#12899,#12900,#12901,#12902,#12903));
#3127=EDGE_LOOP('',(#12904,#12905,#12906,#12907,#12908,#12909));
#3128=EDGE_LOOP('',(#12910,#12911,#12912,#12913,#12914,#12915));
#3129=EDGE_LOOP('',(#12916,#12917,#12918,#12919,#12920,#12921));
#3130=EDGE_LOOP('',(#12922,#12923,#12924,#12925,#12926,#12927));
#3131=EDGE_LOOP('',(#12928,#12929,#12930,#12931,#12932,#12933));
#3132=EDGE_LOOP('',(#12934,#12935,#12936,#12937,#12938,#12939));
#3133=EDGE_LOOP('',(#12940,#12941,#12942,#12943,#12944,#12945));
#3134=EDGE_LOOP('',(#12946,#12947,#12948,#12949,#12950,#12951));
#3135=EDGE_LOOP('',(#12952,#12953,#12954,#12955,#12956,#12957));
#3136=EDGE_LOOP('',(#12958,#12959,#12960,#12961,#12962,#12963));
#3137=EDGE_LOOP('',(#12964,#12965,#12966,#12967,#12968,#12969));
#3138=EDGE_LOOP('',(#12970,#12971,#12972,#12973,#12974,#12975));
#3139=EDGE_LOOP('',(#12976,#12977,#12978,#12979,#12980,#12981));
#3140=EDGE_LOOP('',(#12982,#12983,#12984,#12985,#12986,#12987));
#3141=EDGE_LOOP('',(#12988,#12989,#12990,#12991,#12992,#12993));
#3142=EDGE_LOOP('',(#12994,#12995,#12996,#12997,#12998,#12999));
#3143=EDGE_LOOP('',(#13000,#13001,#13002,#13003,#13004,#13005));
#3144=EDGE_LOOP('',(#13006,#13007,#13008,#13009,#13010,#13011));
#3145=EDGE_LOOP('',(#13012,#13013,#13014,#13015,#13016,#13017));
#3146=EDGE_LOOP('',(#13018,#13019,#13020,#13021,#13022,#13023));
#3147=EDGE_LOOP('',(#13024,#13025,#13026,#13027,#13028,#13029));
#3148=EDGE_LOOP('',(#13030,#13031,#13032,#13033,#13034,#13035));
#3149=EDGE_LOOP('',(#13036,#13037,#13038,#13039,#13040,#13041));
#3150=EDGE_LOOP('',(#13042,#13043,#13044,#13045,#13046,#13047));
#3151=EDGE_LOOP('',(#13048,#13049,#13050,#13051,#13052,#13053));
#3152=EDGE_LOOP('',(#13054,#13055,#13056,#13057,#13058,#13059));
#3153=EDGE_LOOP('',(#13060,#13061,#13062,#13063,#13064,#13065));
#3154=EDGE_LOOP('',(#13066,#13067,#13068,#13069,#13070,#13071));
#3155=EDGE_LOOP('',(#13072,#13073,#13074,#13075,#13076,#13077));
#3156=EDGE_LOOP('',(#13078,#13079,#13080,#13081,#13082,#13083));
#3157=EDGE_LOOP('',(#13084,#13085,#13086,#13087,#13088,#13089));
#3158=EDGE_LOOP('',(#13090,#13091,#13092,#13093,#13094,#13095));
#3159=EDGE_LOOP('',(#13096,#13097,#13098,#13099,#13100,#13101));
#3160=EDGE_LOOP('',(#13102,#13103,#13104,#13105,#13106,#13107));
#3161=EDGE_LOOP('',(#13108,#13109,#13110,#13111,#13112,#13113));
#3162=EDGE_LOOP('',(#13114,#13115,#13116,#13117,#13118,#13119));
#3163=EDGE_LOOP('',(#13120,#13121,#13122,#13123,#13124,#13125));
#3164=EDGE_LOOP('',(#13126,#13127,#13128,#13129,#13130,#13131));
#3165=EDGE_LOOP('',(#13132,#13133,#13134,#13135,#13136,#13137));
#3166=EDGE_LOOP('',(#13138,#13139,#13140,#13141,#13142,#13143));
#3167=EDGE_LOOP('',(#13144,#13145,#13146,#13147,#13148,#13149));
#3168=EDGE_LOOP('',(#13150,#13151,#13152,#13153,#13154,#13155,#13156,#13157,
#13158,#13159,#13160,#13161,#13162,#13163,#13164,#13165,#13166,#13167,#13168,
#13169,#13170,#13171,#13172,#13173,#13174,#13175,#13176,#13177,#13178,#13179,
#13180,#13181,#13182,#13183,#13184,#13185,#13186,#13187,#13188,#13189,#13190,
#13191,#13192,#13193,#13194,#13195,#13196,#13197,#13198,#13199,#13200,#13201,
#13202,#13203,#13204,#13205,#13206,#13207,#13208,#13209,#13210,#13211,#13212,
#13213,#13214,#13215,#13216,#13217,#13218,#13219,#13220,#13221,#13222,#13223,
#13224,#13225,#13226,#13227,#13228,#13229,#13230,#13231,#13232,#13233,#13234,
#13235,#13236,#13237,#13238,#13239,#13240,#13241,#13242,#13243,#13244,#13245,
#13246,#13247,#13248,#13249,#13250,#13251,#13252,#13253,#13254,#13255,#13256,
#13257,#13258,#13259,#13260,#13261,#13262,#13263,#13264,#13265,#13266,#13267,
#13268,#13269,#13270,#13271,#13272,#13273,#13274,#13275,#13276,#13277,#13278,
#13279,#13280,#13281,#13282,#13283,#13284,#13285,#13286,#13287,#13288,#13289,
#13290,#13291,#13292,#13293,#13294,#13295,#13296,#13297,#13298,#13299,#13300,
#13301,#13302,#13303,#13304,#13305,#13306,#13307,#13308,#13309,#13310,#13311,
#13312,#13313,#13314,#13315,#13316,#13317,#13318,#13319,#13320,#13321,#13322,
#13323,#13324,#13325,#13326,#13327,#13328,#13329,#13330,#13331,#13332,#13333,
#13334,#13335,#13336,#13337,#13338,#13339,#13340,#13341,#13342,#13343,#13344,
#13345,#13346,#13347,#13348,#13349,#13350,#13351,#13352,#13353,#13354,#13355,
#13356,#13357,#13358,#13359,#13360,#13361,#13362,#13363,#13364,#13365,#13366,
#13367,#13368,#13369,#13370,#13371,#13372,#13373,#13374,#13375,#13376,#13377,
#13378,#13379,#13380,#13381,#13382,#13383,#13384));
#3169=EDGE_LOOP('',(#13385,#13386,#13387,#13388,#13389,#13390,#13391,#13392,
#13393,#13394,#13395,#13396,#13397,#13398,#13399,#13400,#13401,#13402,#13403,
#13404,#13405,#13406,#13407,#13408,#13409,#13410,#13411,#13412,#13413,#13414,
#13415,#13416,#13417,#13418,#13419,#13420,#13421,#13422,#13423,#13424,#13425,
#13426,#13427,#13428,#13429,#13430,#13431,#13432,#13433,#13434,#13435,#13436,
#13437,#13438,#13439,#13440,#13441,#13442,#13443,#13444,#13445,#13446,#13447,
#13448,#13449,#13450,#13451,#13452,#13453,#13454,#13455,#13456,#13457,#13458,
#13459,#13460,#13461,#13462,#13463,#13464,#13465,#13466,#13467,#13468,#13469,
#13470,#13471,#13472,#13473,#13474,#13475,#13476,#13477,#13478,#13479,#13480,
#13481,#13482,#13483,#13484,#13485,#13486,#13487,#13488,#13489,#13490,#13491,
#13492,#13493,#13494,#13495,#13496,#13497,#13498,#13499,#13500,#13501,#13502,
#13503,#13504,#13505,#13506,#13507,#13508,#13509,#13510,#13511,#13512,#13513,
#13514,#13515,#13516,#13517,#13518,#13519,#13520,#13521,#13522,#13523,#13524,
#13525,#13526,#13527,#13528,#13529,#13530,#13531,#13532,#13533,#13534,#13535,
#13536,#13537,#13538,#13539,#13540,#13541,#13542,#13543,#13544,#13545,#13546,
#13547,#13548,#13549,#13550,#13551,#13552,#13553,#13554,#13555,#13556,#13557,
#13558,#13559,#13560,#13561,#13562,#13563,#13564,#13565,#13566,#13567,#13568,
#13569,#13570,#13571,#13572,#13573,#13574,#13575,#13576,#13577,#13578,#13579,
#13580,#13581,#13582,#13583,#13584,#13585,#13586,#13587,#13588,#13589,#13590,
#13591,#13592,#13593,#13594,#13595,#13596,#13597,#13598,#13599,#13600,#13601,
#13602,#13603,#13604,#13605,#13606,#13607,#13608,#13609,#13610,#13611,#13612,
#13613,#13614,#13615,#13616,#13617,#13618,#13619));
#3170=EDGE_LOOP('',(#13620,#13621,#13622,#13623,#13624));
#3171=EDGE_LOOP('',(#13625,#13626,#13627,#13628));
#3172=EDGE_LOOP('',(#13629,#13630,#13631,#13632));
#3173=EDGE_LOOP('',(#13633,#13634,#13635,#13636));
#3174=EDGE_LOOP('',(#13637,#13638,#13639,#13640));
#3175=EDGE_LOOP('',(#13641,#13642,#13643,#13644));
#3176=EDGE_LOOP('',(#13645,#13646,#13647,#13648));
#3177=EDGE_LOOP('',(#13649,#13650,#13651,#13652));
#3178=EDGE_LOOP('',(#13653,#13654,#13655,#13656));
#3179=EDGE_LOOP('',(#13657,#13658,#13659,#13660));
#3180=EDGE_LOOP('',(#13661,#13662,#13663,#13664));
#3181=EDGE_LOOP('',(#13665,#13666,#13667,#13668));
#3182=EDGE_LOOP('',(#13669,#13670,#13671,#13672));
#3183=EDGE_LOOP('',(#13673,#13674,#13675,#13676));
#3184=EDGE_LOOP('',(#13677,#13678,#13679,#13680));
#3185=EDGE_LOOP('',(#13681,#13682,#13683,#13684));
#3186=EDGE_LOOP('',(#13685,#13686,#13687,#13688));
#3187=EDGE_LOOP('',(#13689,#13690,#13691,#13692));
#3188=EDGE_LOOP('',(#13693,#13694,#13695,#13696));
#3189=EDGE_LOOP('',(#13697,#13698,#13699,#13700));
#3190=EDGE_LOOP('',(#13701,#13702,#13703,#13704));
#3191=EDGE_LOOP('',(#13705,#13706,#13707,#13708));
#3192=EDGE_LOOP('',(#13709,#13710,#13711,#13712));
#3193=EDGE_LOOP('',(#13713,#13714,#13715,#13716));
#3194=EDGE_LOOP('',(#13717,#13718,#13719,#13720));
#3195=EDGE_LOOP('',(#13721,#13722,#13723,#13724));
#3196=EDGE_LOOP('',(#13725,#13726,#13727,#13728));
#3197=EDGE_LOOP('',(#13729,#13730,#13731,#13732));
#3198=EDGE_LOOP('',(#13733,#13734,#13735,#13736));
#3199=EDGE_LOOP('',(#13737,#13738,#13739,#13740));
#3200=EDGE_LOOP('',(#13741,#13742,#13743,#13744));
#3201=EDGE_LOOP('',(#13745,#13746,#13747,#13748));
#3202=EDGE_LOOP('',(#13749,#13750,#13751,#13752));
#3203=EDGE_LOOP('',(#13753,#13754,#13755,#13756));
#3204=EDGE_LOOP('',(#13757,#13758,#13759,#13760));
#3205=EDGE_LOOP('',(#13761,#13762,#13763,#13764));
#3206=EDGE_LOOP('',(#13765,#13766,#13767,#13768));
#3207=EDGE_LOOP('',(#13769,#13770,#13771,#13772));
#3208=EDGE_LOOP('',(#13773,#13774,#13775,#13776));
#3209=EDGE_LOOP('',(#13777,#13778,#13779,#13780));
#3210=EDGE_LOOP('',(#13781,#13782,#13783,#13784));
#3211=EDGE_LOOP('',(#13785,#13786,#13787,#13788));
#3212=EDGE_LOOP('',(#13789,#13790,#13791,#13792));
#3213=EDGE_LOOP('',(#13793,#13794,#13795,#13796));
#3214=EDGE_LOOP('',(#13797,#13798,#13799,#13800));
#3215=EDGE_LOOP('',(#13801,#13802,#13803,#13804));
#3216=EDGE_LOOP('',(#13805,#13806,#13807,#13808));
#3217=EDGE_LOOP('',(#13809,#13810,#13811,#13812));
#3218=EDGE_LOOP('',(#13813,#13814,#13815,#13816));
#3219=EDGE_LOOP('',(#13817,#13818,#13819,#13820));
#3220=EDGE_LOOP('',(#13821,#13822,#13823,#13824));
#3221=EDGE_LOOP('',(#13825,#13826,#13827,#13828));
#3222=EDGE_LOOP('',(#13829,#13830,#13831,#13832));
#3223=EDGE_LOOP('',(#13833,#13834,#13835,#13836));
#3224=EDGE_LOOP('',(#13837,#13838,#13839,#13840));
#3225=EDGE_LOOP('',(#13841,#13842,#13843,#13844));
#3226=EDGE_LOOP('',(#13845,#13846,#13847,#13848));
#3227=EDGE_LOOP('',(#13849,#13850,#13851,#13852));
#3228=EDGE_LOOP('',(#13853,#13854,#13855,#13856));
#3229=EDGE_LOOP('',(#13857,#13858,#13859,#13860));
#3230=EDGE_LOOP('',(#13861,#13862,#13863,#13864));
#3231=EDGE_LOOP('',(#13865,#13866,#13867,#13868));
#3232=EDGE_LOOP('',(#13869,#13870,#13871,#13872));
#3233=EDGE_LOOP('',(#13873,#13874,#13875,#13876));
#3234=EDGE_LOOP('',(#13877,#13878,#13879,#13880));
#3235=EDGE_LOOP('',(#13881,#13882,#13883,#13884));
#3236=EDGE_LOOP('',(#13885,#13886,#13887,#13888));
#3237=EDGE_LOOP('',(#13889,#13890,#13891,#13892));
#3238=EDGE_LOOP('',(#13893,#13894,#13895,#13896));
#3239=EDGE_LOOP('',(#13897,#13898,#13899,#13900));
#3240=EDGE_LOOP('',(#13901,#13902,#13903,#13904));
#3241=EDGE_LOOP('',(#13905,#13906,#13907,#13908));
#3242=EDGE_LOOP('',(#13909,#13910,#13911,#13912));
#3243=EDGE_LOOP('',(#13913,#13914,#13915,#13916));
#3244=EDGE_LOOP('',(#13917,#13918,#13919,#13920));
#3245=EDGE_LOOP('',(#13921,#13922,#13923,#13924));
#3246=EDGE_LOOP('',(#13925,#13926,#13927,#13928));
#3247=EDGE_LOOP('',(#13929));
#3248=EDGE_LOOP('',(#13930));
#3249=EDGE_LOOP('',(#13931,#13932,#13933,#13934));
#3250=EDGE_LOOP('',(#13935));
#3251=EDGE_LOOP('',(#13936));
#3252=EDGE_LOOP('',(#13937,#13938,#13939,#13940));
#3253=EDGE_LOOP('',(#13941,#13942,#13943,#13944));
#3254=EDGE_LOOP('',(#13945,#13946,#13947,#13948));
#3255=EDGE_LOOP('',(#13949,#13950,#13951,#13952));
#3256=EDGE_LOOP('',(#13953,#13954,#13955,#13956));
#3257=EDGE_LOOP('',(#13957,#13958,#13959,#13960));
#3258=EDGE_LOOP('',(#13961,#13962,#13963,#13964));
#3259=EDGE_LOOP('',(#13965,#13966,#13967,#13968));
#3260=EDGE_LOOP('',(#13969,#13970,#13971,#13972));
#3261=EDGE_LOOP('',(#13973,#13974,#13975,#13976));
#3262=EDGE_LOOP('',(#13977,#13978,#13979,#13980));
#3263=EDGE_LOOP('',(#13981,#13982,#13983,#13984));
#3264=EDGE_LOOP('',(#13985,#13986,#13987,#13988));
#3265=EDGE_LOOP('',(#13989,#13990,#13991,#13992));
#3266=EDGE_LOOP('',(#13993,#13994,#13995,#13996));
#3267=EDGE_LOOP('',(#13997,#13998,#13999,#14000));
#3268=EDGE_LOOP('',(#14001,#14002,#14003,#14004));
#3269=EDGE_LOOP('',(#14005,#14006,#14007,#14008));
#3270=EDGE_LOOP('',(#14009,#14010,#14011,#14012));
#3271=EDGE_LOOP('',(#14013,#14014,#14015,#14016));
#3272=EDGE_LOOP('',(#14017,#14018,#14019,#14020));
#3273=EDGE_LOOP('',(#14021,#14022,#14023,#14024));
#3274=EDGE_LOOP('',(#14025,#14026,#14027,#14028));
#3275=EDGE_LOOP('',(#14029,#14030,#14031,#14032));
#3276=EDGE_LOOP('',(#14033,#14034,#14035,#14036));
#3277=EDGE_LOOP('',(#14037,#14038,#14039,#14040));
#3278=EDGE_LOOP('',(#14041,#14042,#14043,#14044));
#3279=EDGE_LOOP('',(#14045,#14046,#14047,#14048));
#3280=EDGE_LOOP('',(#14049,#14050,#14051,#14052));
#3281=EDGE_LOOP('',(#14053,#14054,#14055,#14056));
#3282=EDGE_LOOP('',(#14057,#14058,#14059,#14060));
#3283=EDGE_LOOP('',(#14061,#14062,#14063,#14064));
#3284=EDGE_LOOP('',(#14065,#14066,#14067,#14068));
#3285=EDGE_LOOP('',(#14069,#14070,#14071,#14072));
#3286=EDGE_LOOP('',(#14073,#14074,#14075,#14076));
#3287=EDGE_LOOP('',(#14077,#14078,#14079,#14080));
#3288=EDGE_LOOP('',(#14081,#14082,#14083,#14084));
#3289=EDGE_LOOP('',(#14085,#14086,#14087,#14088));
#3290=EDGE_LOOP('',(#14089,#14090,#14091,#14092));
#3291=EDGE_LOOP('',(#14093,#14094,#14095,#14096));
#3292=EDGE_LOOP('',(#14097,#14098,#14099,#14100,#14101));
#3293=EDGE_LOOP('',(#14102,#14103,#14104,#14105));
#3294=EDGE_LOOP('',(#14106,#14107,#14108,#14109));
#3295=EDGE_LOOP('',(#14110,#14111,#14112,#14113));
#3296=EDGE_LOOP('',(#14114,#14115,#14116,#14117));
#3297=EDGE_LOOP('',(#14118,#14119,#14120,#14121));
#3298=EDGE_LOOP('',(#14122,#14123,#14124,#14125));
#3299=EDGE_LOOP('',(#14126,#14127,#14128,#14129));
#3300=EDGE_LOOP('',(#14130,#14131,#14132,#14133));
#3301=EDGE_LOOP('',(#14134,#14135,#14136,#14137));
#3302=EDGE_LOOP('',(#14138,#14139,#14140,#14141));
#3303=EDGE_LOOP('',(#14142,#14143,#14144,#14145));
#3304=EDGE_LOOP('',(#14146,#14147,#14148,#14149));
#3305=EDGE_LOOP('',(#14150,#14151,#14152,#14153));
#3306=EDGE_LOOP('',(#14154,#14155,#14156,#14157));
#3307=EDGE_LOOP('',(#14158,#14159,#14160,#14161));
#3308=EDGE_LOOP('',(#14162,#14163,#14164,#14165));
#3309=EDGE_LOOP('',(#14166,#14167,#14168,#14169));
#3310=EDGE_LOOP('',(#14170,#14171,#14172,#14173));
#3311=EDGE_LOOP('',(#14174,#14175,#14176,#14177));
#3312=EDGE_LOOP('',(#14178,#14179,#14180,#14181));
#3313=EDGE_LOOP('',(#14182,#14183,#14184,#14185));
#3314=EDGE_LOOP('',(#14186,#14187,#14188,#14189));
#3315=EDGE_LOOP('',(#14190,#14191,#14192,#14193));
#3316=EDGE_LOOP('',(#14194,#14195,#14196,#14197));
#3317=EDGE_LOOP('',(#14198,#14199,#14200,#14201));
#3318=EDGE_LOOP('',(#14202,#14203,#14204,#14205));
#3319=EDGE_LOOP('',(#14206,#14207,#14208,#14209));
#3320=EDGE_LOOP('',(#14210,#14211,#14212,#14213));
#3321=EDGE_LOOP('',(#14214,#14215,#14216,#14217));
#3322=EDGE_LOOP('',(#14218,#14219,#14220,#14221));
#3323=EDGE_LOOP('',(#14222,#14223,#14224,#14225));
#3324=EDGE_LOOP('',(#14226,#14227,#14228,#14229));
#3325=EDGE_LOOP('',(#14230,#14231,#14232,#14233));
#3326=EDGE_LOOP('',(#14234,#14235,#14236,#14237));
#3327=EDGE_LOOP('',(#14238,#14239,#14240,#14241));
#3328=EDGE_LOOP('',(#14242,#14243,#14244,#14245));
#3329=EDGE_LOOP('',(#14246,#14247,#14248,#14249));
#3330=EDGE_LOOP('',(#14250,#14251,#14252,#14253));
#3331=EDGE_LOOP('',(#14254,#14255,#14256,#14257));
#3332=EDGE_LOOP('',(#14258,#14259,#14260,#14261));
#3333=EDGE_LOOP('',(#14262,#14263,#14264,#14265));
#3334=EDGE_LOOP('',(#14266,#14267,#14268,#14269));
#3335=EDGE_LOOP('',(#14270,#14271,#14272,#14273));
#3336=EDGE_LOOP('',(#14274,#14275,#14276,#14277));
#3337=EDGE_LOOP('',(#14278,#14279,#14280,#14281));
#3338=EDGE_LOOP('',(#14282,#14283,#14284,#14285));
#3339=EDGE_LOOP('',(#14286,#14287,#14288,#14289));
#3340=EDGE_LOOP('',(#14290,#14291,#14292,#14293));
#3341=EDGE_LOOP('',(#14294,#14295,#14296,#14297));
#3342=EDGE_LOOP('',(#14298,#14299,#14300,#14301));
#3343=EDGE_LOOP('',(#14302,#14303,#14304,#14305));
#3344=EDGE_LOOP('',(#14306,#14307,#14308,#14309));
#3345=EDGE_LOOP('',(#14310,#14311,#14312,#14313));
#3346=EDGE_LOOP('',(#14314,#14315,#14316,#14317));
#3347=EDGE_LOOP('',(#14318,#14319,#14320,#14321));
#3348=EDGE_LOOP('',(#14322,#14323,#14324,#14325));
#3349=EDGE_LOOP('',(#14326,#14327,#14328,#14329));
#3350=EDGE_LOOP('',(#14330,#14331,#14332,#14333));
#3351=EDGE_LOOP('',(#14334,#14335,#14336,#14337));
#3352=EDGE_LOOP('',(#14338,#14339,#14340,#14341));
#3353=EDGE_LOOP('',(#14342,#14343,#14344,#14345));
#3354=EDGE_LOOP('',(#14346,#14347,#14348,#14349));
#3355=EDGE_LOOP('',(#14350,#14351,#14352,#14353));
#3356=EDGE_LOOP('',(#14354,#14355,#14356,#14357));
#3357=EDGE_LOOP('',(#14358,#14359,#14360,#14361));
#3358=EDGE_LOOP('',(#14362,#14363,#14364,#14365));
#3359=EDGE_LOOP('',(#14366,#14367,#14368,#14369));
#3360=EDGE_LOOP('',(#14370,#14371,#14372,#14373));
#3361=EDGE_LOOP('',(#14374,#14375,#14376,#14377));
#3362=EDGE_LOOP('',(#14378,#14379,#14380,#14381));
#3363=EDGE_LOOP('',(#14382,#14383,#14384,#14385));
#3364=EDGE_LOOP('',(#14386,#14387,#14388,#14389));
#3365=EDGE_LOOP('',(#14390,#14391,#14392,#14393));
#3366=EDGE_LOOP('',(#14394,#14395,#14396,#14397));
#3367=EDGE_LOOP('',(#14398,#14399,#14400,#14401));
#3368=EDGE_LOOP('',(#14402,#14403,#14404,#14405));
#3369=EDGE_LOOP('',(#14406,#14407,#14408,#14409));
#3370=EDGE_LOOP('',(#14410,#14411,#14412,#14413));
#3371=EDGE_LOOP('',(#14414,#14415,#14416,#14417,#14418));
#3372=EDGE_LOOP('',(#14419,#14420,#14421,#14422));
#3373=EDGE_LOOP('',(#14423,#14424,#14425,#14426));
#3374=EDGE_LOOP('',(#14427,#14428,#14429,#14430));
#3375=EDGE_LOOP('',(#14431,#14432,#14433,#14434));
#3376=EDGE_LOOP('',(#14435,#14436,#14437,#14438));
#3377=EDGE_LOOP('',(#14439,#14440,#14441,#14442));
#3378=EDGE_LOOP('',(#14443,#14444,#14445,#14446));
#3379=EDGE_LOOP('',(#14447,#14448,#14449,#14450));
#3380=EDGE_LOOP('',(#14451,#14452,#14453,#14454));
#3381=EDGE_LOOP('',(#14455,#14456,#14457,#14458));
#3382=EDGE_LOOP('',(#14459,#14460,#14461,#14462));
#3383=EDGE_LOOP('',(#14463,#14464,#14465,#14466));
#3384=EDGE_LOOP('',(#14467,#14468,#14469,#14470));
#3385=EDGE_LOOP('',(#14471,#14472,#14473,#14474));
#3386=EDGE_LOOP('',(#14475,#14476,#14477,#14478));
#3387=EDGE_LOOP('',(#14479,#14480,#14481,#14482));
#3388=EDGE_LOOP('',(#14483,#14484,#14485,#14486));
#3389=EDGE_LOOP('',(#14487,#14488,#14489,#14490));
#3390=EDGE_LOOP('',(#14491,#14492,#14493,#14494));
#3391=EDGE_LOOP('',(#14495,#14496,#14497,#14498));
#3392=EDGE_LOOP('',(#14499,#14500,#14501,#14502));
#3393=EDGE_LOOP('',(#14503,#14504,#14505,#14506));
#3394=EDGE_LOOP('',(#14507,#14508,#14509,#14510));
#3395=EDGE_LOOP('',(#14511,#14512,#14513,#14514));
#3396=EDGE_LOOP('',(#14515,#14516,#14517,#14518));
#3397=EDGE_LOOP('',(#14519,#14520,#14521,#14522));
#3398=EDGE_LOOP('',(#14523,#14524,#14525,#14526));
#3399=EDGE_LOOP('',(#14527,#14528,#14529,#14530));
#3400=EDGE_LOOP('',(#14531,#14532,#14533,#14534));
#3401=EDGE_LOOP('',(#14535,#14536,#14537,#14538));
#3402=EDGE_LOOP('',(#14539,#14540,#14541,#14542));
#3403=EDGE_LOOP('',(#14543,#14544,#14545,#14546));
#3404=EDGE_LOOP('',(#14547,#14548,#14549,#14550));
#3405=EDGE_LOOP('',(#14551,#14552,#14553,#14554));
#3406=EDGE_LOOP('',(#14555,#14556,#14557,#14558,#14559,#14560,#14561,#14562,
#14563,#14564,#14565,#14566,#14567));
#3407=EDGE_LOOP('',(#14568,#14569,#14570,#14571,#14572));
#3408=EDGE_LOOP('',(#14573,#14574,#14575,#14576));
#3409=EDGE_LOOP('',(#14577,#14578));
#3410=EDGE_LOOP('',(#14579));
#3411=EDGE_LOOP('',(#14580,#14581));
#3412=EDGE_LOOP('',(#14582));
#3413=EDGE_LOOP('',(#14583));
#3414=EDGE_LOOP('',(#14584,#14585,#14586,#14587));
#3415=EDGE_LOOP('',(#14588,#14589,#14590,#14591));
#3416=EDGE_LOOP('',(#14592,#14593,#14594,#14595,#14596));
#3417=EDGE_LOOP('',(#14597,#14598,#14599,#14600));
#3418=EDGE_LOOP('',(#14601,#14602,#14603,#14604,#14605));
#3419=EDGE_LOOP('',(#14606,#14607,#14608,#14609,#14610,#14611));
#3420=EDGE_LOOP('',(#14612,#14613,#14614,#14615,#14616,#14617));
#3421=EDGE_LOOP('',(#14618,#14619,#14620,#14621,#14622,#14623));
#3422=EDGE_LOOP('',(#14624,#14625,#14626,#14627,#14628,#14629));
#3423=EDGE_LOOP('',(#14630,#14631,#14632,#14633,#14634,#14635));
#3424=EDGE_LOOP('',(#14636,#14637,#14638,#14639,#14640,#14641));
#3425=EDGE_LOOP('',(#14642,#14643,#14644,#14645,#14646,#14647));
#3426=EDGE_LOOP('',(#14648,#14649,#14650,#14651,#14652,#14653));
#3427=EDGE_LOOP('',(#14654,#14655,#14656,#14657,#14658,#14659));
#3428=EDGE_LOOP('',(#14660,#14661,#14662,#14663,#14664,#14665));
#3429=EDGE_LOOP('',(#14666,#14667,#14668,#14669,#14670,#14671));
#3430=EDGE_LOOP('',(#14672,#14673,#14674,#14675,#14676,#14677));
#3431=EDGE_LOOP('',(#14678,#14679,#14680,#14681,#14682,#14683));
#3432=EDGE_LOOP('',(#14684,#14685,#14686,#14687,#14688,#14689));
#3433=EDGE_LOOP('',(#14690,#14691,#14692,#14693,#14694,#14695));
#3434=EDGE_LOOP('',(#14696,#14697,#14698,#14699,#14700,#14701));
#3435=EDGE_LOOP('',(#14702,#14703,#14704,#14705,#14706,#14707));
#3436=EDGE_LOOP('',(#14708,#14709,#14710,#14711,#14712,#14713));
#3437=EDGE_LOOP('',(#14714,#14715,#14716,#14717,#14718,#14719));
#3438=EDGE_LOOP('',(#14720,#14721,#14722,#14723,#14724,#14725));
#3439=EDGE_LOOP('',(#14726,#14727,#14728,#14729,#14730,#14731));
#3440=EDGE_LOOP('',(#14732,#14733,#14734,#14735,#14736,#14737));
#3441=EDGE_LOOP('',(#14738,#14739,#14740,#14741,#14742,#14743));
#3442=EDGE_LOOP('',(#14744,#14745,#14746,#14747,#14748,#14749));
#3443=EDGE_LOOP('',(#14750,#14751,#14752,#14753,#14754,#14755));
#3444=EDGE_LOOP('',(#14756,#14757,#14758,#14759,#14760,#14761));
#3445=EDGE_LOOP('',(#14762,#14763,#14764,#14765,#14766,#14767));
#3446=EDGE_LOOP('',(#14768,#14769,#14770,#14771,#14772,#14773));
#3447=EDGE_LOOP('',(#14774,#14775,#14776,#14777,#14778,#14779));
#3448=EDGE_LOOP('',(#14780,#14781,#14782,#14783,#14784,#14785));
#3449=EDGE_LOOP('',(#14786,#14787,#14788,#14789,#14790,#14791));
#3450=EDGE_LOOP('',(#14792,#14793,#14794,#14795,#14796,#14797));
#3451=EDGE_LOOP('',(#14798,#14799,#14800,#14801,#14802,#14803));
#3452=EDGE_LOOP('',(#14804,#14805,#14806,#14807,#14808,#14809));
#3453=EDGE_LOOP('',(#14810,#14811,#14812,#14813,#14814,#14815));
#3454=EDGE_LOOP('',(#14816,#14817,#14818,#14819,#14820,#14821));
#3455=EDGE_LOOP('',(#14822,#14823,#14824,#14825,#14826,#14827));
#3456=EDGE_LOOP('',(#14828,#14829,#14830,#14831,#14832,#14833));
#3457=EDGE_LOOP('',(#14834,#14835,#14836,#14837));
#3458=EDGE_LOOP('',(#14838,#14839,#14840,#14841,#14842,#14843,#14844,#14845,
#14846,#14847,#14848,#14849,#14850,#14851,#14852,#14853,#14854,#14855,#14856,
#14857,#14858,#14859,#14860,#14861,#14862,#14863,#14864,#14865,#14866,#14867,
#14868,#14869,#14870,#14871,#14872,#14873,#14874,#14875,#14876,#14877,#14878,
#14879,#14880,#14881,#14882,#14883,#14884,#14885,#14886,#14887,#14888,#14889,
#14890,#14891,#14892,#14893,#14894,#14895,#14896,#14897,#14898,#14899,#14900,
#14901,#14902,#14903,#14904,#14905,#14906,#14907,#14908,#14909,#14910,#14911,
#14912,#14913,#14914,#14915,#14916,#14917,#14918,#14919,#14920,#14921,#14922,
#14923,#14924,#14925,#14926,#14927,#14928,#14929,#14930,#14931,#14932,#14933,
#14934,#14935,#14936,#14937,#14938,#14939,#14940,#14941,#14942,#14943,#14944,
#14945,#14946,#14947,#14948,#14949,#14950,#14951,#14952,#14953,#14954,#14955,
#14956,#14957,#14958,#14959,#14960,#14961,#14962,#14963,#14964,#14965,#14966,
#14967,#14968,#14969,#14970,#14971,#14972,#14973,#14974,#14975,#14976,#14977,
#14978,#14979,#14980,#14981,#14982,#14983,#14984,#14985,#14986,#14987,#14988,
#14989,#14990,#14991,#14992,#14993,#14994,#14995,#14996,#14997,#14998,#14999,
#15000,#15001,#15002,#15003,#15004,#15005,#15006,#15007,#15008,#15009,#15010,
#15011,#15012,#15013,#15014,#15015,#15016,#15017,#15018,#15019,#15020,#15021,
#15022,#15023,#15024,#15025,#15026,#15027,#15028,#15029,#15030,#15031,#15032,
#15033,#15034,#15035,#15036,#15037,#15038,#15039,#15040,#15041,#15042,#15043,
#15044,#15045,#15046,#15047,#15048,#15049,#15050,#15051,#15052,#15053,#15054,
#15055,#15056,#15057,#15058,#15059,#15060,#15061,#15062,#15063,#15064,#15065,
#15066,#15067,#15068,#15069,#15070,#15071,#15072));
#3459=EDGE_LOOP('',(#15073,#15074,#15075,#15076,#15077,#15078,#15079,#15080,
#15081,#15082,#15083,#15084,#15085,#15086,#15087,#15088,#15089,#15090,#15091,
#15092,#15093,#15094,#15095,#15096,#15097,#15098,#15099,#15100,#15101,#15102,
#15103,#15104,#15105,#15106,#15107,#15108,#15109,#15110,#15111,#15112,#15113,
#15114,#15115,#15116,#15117,#15118,#15119,#15120,#15121,#15122,#15123,#15124,
#15125,#15126,#15127,#15128,#15129,#15130,#15131,#15132,#15133,#15134,#15135,
#15136,#15137,#15138,#15139,#15140,#15141,#15142,#15143,#15144,#15145,#15146,
#15147,#15148,#15149,#15150,#15151,#15152,#15153,#15154,#15155,#15156,#15157,
#15158,#15159,#15160,#15161,#15162,#15163,#15164,#15165,#15166,#15167,#15168,
#15169,#15170,#15171,#15172,#15173,#15174,#15175,#15176,#15177,#15178,#15179,
#15180,#15181,#15182,#15183,#15184,#15185,#15186,#15187,#15188,#15189,#15190,
#15191,#15192,#15193,#15194,#15195,#15196,#15197,#15198,#15199,#15200,#15201,
#15202,#15203,#15204,#15205,#15206,#15207,#15208,#15209,#15210,#15211,#15212,
#15213,#15214,#15215,#15216,#15217,#15218,#15219,#15220,#15221,#15222,#15223,
#15224,#15225,#15226,#15227,#15228,#15229,#15230,#15231,#15232,#15233,#15234,
#15235,#15236,#15237,#15238,#15239,#15240,#15241,#15242,#15243,#15244,#15245,
#15246,#15247,#15248,#15249,#15250,#15251,#15252,#15253,#15254,#15255,#15256,
#15257,#15258,#15259,#15260,#15261,#15262,#15263,#15264,#15265,#15266,#15267,
#15268,#15269,#15270,#15271,#15272,#15273,#15274,#15275,#15276,#15277,#15278,
#15279,#15280,#15281,#15282,#15283,#15284,#15285,#15286,#15287,#15288,#15289,
#15290,#15291,#15292,#15293,#15294,#15295,#15296,#15297,#15298,#15299,#15300,
#15301,#15302,#15303,#15304,#15305,#15306,#15307));
#3460=EDGE_LOOP('',(#15308,#15309,#15310,#15311,#15312));
#3461=EDGE_LOOP('',(#15313,#15314,#15315,#15316));
#3462=EDGE_LOOP('',(#15317,#15318,#15319,#15320));
#3463=EDGE_LOOP('',(#15321,#15322,#15323,#15324));
#3464=EDGE_LOOP('',(#15325,#15326,#15327,#15328));
#3465=EDGE_LOOP('',(#15329,#15330,#15331,#15332));
#3466=EDGE_LOOP('',(#15333,#15334,#15335,#15336));
#3467=EDGE_LOOP('',(#15337,#15338,#15339,#15340));
#3468=EDGE_LOOP('',(#15341,#15342,#15343,#15344));
#3469=EDGE_LOOP('',(#15345,#15346,#15347,#15348));
#3470=EDGE_LOOP('',(#15349,#15350,#15351,#15352));
#3471=EDGE_LOOP('',(#15353,#15354,#15355,#15356));
#3472=EDGE_LOOP('',(#15357,#15358,#15359,#15360));
#3473=EDGE_LOOP('',(#15361,#15362,#15363,#15364));
#3474=EDGE_LOOP('',(#15365,#15366,#15367,#15368));
#3475=EDGE_LOOP('',(#15369,#15370,#15371,#15372));
#3476=EDGE_LOOP('',(#15373,#15374,#15375,#15376));
#3477=EDGE_LOOP('',(#15377,#15378,#15379,#15380));
#3478=EDGE_LOOP('',(#15381,#15382,#15383,#15384));
#3479=EDGE_LOOP('',(#15385,#15386,#15387,#15388));
#3480=EDGE_LOOP('',(#15389,#15390,#15391,#15392));
#3481=EDGE_LOOP('',(#15393,#15394,#15395,#15396));
#3482=EDGE_LOOP('',(#15397,#15398,#15399,#15400));
#3483=EDGE_LOOP('',(#15401,#15402,#15403,#15404));
#3484=EDGE_LOOP('',(#15405,#15406,#15407,#15408));
#3485=EDGE_LOOP('',(#15409,#15410,#15411,#15412));
#3486=EDGE_LOOP('',(#15413,#15414,#15415,#15416));
#3487=EDGE_LOOP('',(#15417,#15418,#15419,#15420));
#3488=EDGE_LOOP('',(#15421,#15422,#15423,#15424));
#3489=EDGE_LOOP('',(#15425,#15426,#15427,#15428));
#3490=EDGE_LOOP('',(#15429,#15430,#15431,#15432));
#3491=EDGE_LOOP('',(#15433,#15434,#15435,#15436));
#3492=EDGE_LOOP('',(#15437,#15438,#15439,#15440));
#3493=EDGE_LOOP('',(#15441,#15442,#15443,#15444));
#3494=EDGE_LOOP('',(#15445,#15446,#15447,#15448));
#3495=EDGE_LOOP('',(#15449,#15450,#15451,#15452));
#3496=EDGE_LOOP('',(#15453,#15454,#15455,#15456));
#3497=EDGE_LOOP('',(#15457,#15458,#15459,#15460));
#3498=EDGE_LOOP('',(#15461,#15462,#15463,#15464));
#3499=EDGE_LOOP('',(#15465,#15466,#15467,#15468));
#3500=EDGE_LOOP('',(#15469,#15470,#15471,#15472));
#3501=EDGE_LOOP('',(#15473,#15474,#15475,#15476));
#3502=EDGE_LOOP('',(#15477,#15478,#15479,#15480));
#3503=EDGE_LOOP('',(#15481,#15482,#15483,#15484));
#3504=EDGE_LOOP('',(#15485,#15486,#15487,#15488));
#3505=EDGE_LOOP('',(#15489,#15490,#15491,#15492));
#3506=EDGE_LOOP('',(#15493,#15494,#15495,#15496));
#3507=EDGE_LOOP('',(#15497,#15498,#15499,#15500));
#3508=EDGE_LOOP('',(#15501,#15502,#15503,#15504));
#3509=EDGE_LOOP('',(#15505,#15506,#15507,#15508));
#3510=EDGE_LOOP('',(#15509,#15510,#15511,#15512));
#3511=EDGE_LOOP('',(#15513,#15514,#15515,#15516));
#3512=EDGE_LOOP('',(#15517,#15518,#15519,#15520));
#3513=EDGE_LOOP('',(#15521,#15522,#15523,#15524));
#3514=EDGE_LOOP('',(#15525,#15526,#15527,#15528));
#3515=EDGE_LOOP('',(#15529,#15530,#15531,#15532));
#3516=EDGE_LOOP('',(#15533,#15534,#15535,#15536));
#3517=EDGE_LOOP('',(#15537,#15538,#15539,#15540));
#3518=EDGE_LOOP('',(#15541,#15542,#15543,#15544));
#3519=EDGE_LOOP('',(#15545,#15546,#15547,#15548));
#3520=EDGE_LOOP('',(#15549,#15550,#15551,#15552));
#3521=EDGE_LOOP('',(#15553,#15554,#15555,#15556));
#3522=EDGE_LOOP('',(#15557,#15558,#15559,#15560));
#3523=EDGE_LOOP('',(#15561,#15562,#15563,#15564));
#3524=EDGE_LOOP('',(#15565,#15566,#15567,#15568));
#3525=EDGE_LOOP('',(#15569,#15570,#15571,#15572));
#3526=EDGE_LOOP('',(#15573,#15574,#15575,#15576));
#3527=EDGE_LOOP('',(#15577,#15578,#15579,#15580));
#3528=EDGE_LOOP('',(#15581,#15582,#15583,#15584));
#3529=EDGE_LOOP('',(#15585,#15586,#15587,#15588));
#3530=EDGE_LOOP('',(#15589,#15590,#15591,#15592));
#3531=EDGE_LOOP('',(#15593,#15594,#15595,#15596));
#3532=EDGE_LOOP('',(#15597,#15598,#15599,#15600));
#3533=EDGE_LOOP('',(#15601,#15602,#15603,#15604));
#3534=EDGE_LOOP('',(#15605,#15606,#15607,#15608));
#3535=EDGE_LOOP('',(#15609,#15610,#15611,#15612));
#3536=EDGE_LOOP('',(#15613,#15614,#15615,#15616));
#3537=EDGE_LOOP('',(#15617));
#3538=EDGE_LOOP('',(#15618,#15619,#15620,#15621));
#3539=EDGE_LOOP('',(#15622));
#3540=EDGE_LOOP('',(#15623));
#3541=EDGE_LOOP('',(#15624));
#3542=EDGE_LOOP('',(#15625));
#3543=EDGE_LOOP('',(#15626));
#3544=EDGE_LOOP('',(#15627,#15628,#15629,#15630));
#3545=EDGE_LOOP('',(#15631,#15632,#15633,#15634));
#3546=EDGE_LOOP('',(#15635,#15636,#15637,#15638));
#3547=EDGE_LOOP('',(#15639,#15640,#15641,#15642));
#3548=EDGE_LOOP('',(#15643,#15644,#15645,#15646));
#3549=EDGE_LOOP('',(#15647,#15648,#15649,#15650));
#3550=EDGE_LOOP('',(#15651,#15652,#15653,#15654));
#3551=EDGE_LOOP('',(#15655,#15656,#15657,#15658));
#3552=EDGE_LOOP('',(#15659,#15660,#15661,#15662));
#3553=EDGE_LOOP('',(#15663,#15664,#15665,#15666));
#3554=EDGE_LOOP('',(#15667,#15668,#15669,#15670));
#3555=EDGE_LOOP('',(#15671,#15672,#15673,#15674));
#3556=EDGE_LOOP('',(#15675,#15676,#15677,#15678));
#3557=EDGE_LOOP('',(#15679,#15680,#15681,#15682));
#3558=EDGE_LOOP('',(#15683,#15684,#15685,#15686));
#3559=EDGE_LOOP('',(#15687,#15688,#15689,#15690));
#3560=EDGE_LOOP('',(#15691,#15692,#15693,#15694));
#3561=EDGE_LOOP('',(#15695,#15696,#15697,#15698));
#3562=EDGE_LOOP('',(#15699,#15700,#15701,#15702));
#3563=EDGE_LOOP('',(#15703,#15704,#15705,#15706));
#3564=EDGE_LOOP('',(#15707,#15708,#15709,#15710));
#3565=EDGE_LOOP('',(#15711,#15712,#15713,#15714));
#3566=EDGE_LOOP('',(#15715,#15716,#15717,#15718));
#3567=EDGE_LOOP('',(#15719,#15720,#15721,#15722));
#3568=EDGE_LOOP('',(#15723,#15724,#15725,#15726));
#3569=EDGE_LOOP('',(#15727,#15728,#15729,#15730));
#3570=EDGE_LOOP('',(#15731,#15732,#15733,#15734));
#3571=EDGE_LOOP('',(#15735,#15736,#15737,#15738));
#3572=EDGE_LOOP('',(#15739,#15740,#15741,#15742));
#3573=EDGE_LOOP('',(#15743,#15744,#15745,#15746));
#3574=EDGE_LOOP('',(#15747,#15748,#15749,#15750));
#3575=EDGE_LOOP('',(#15751,#15752,#15753,#15754));
#3576=EDGE_LOOP('',(#15755,#15756,#15757,#15758));
#3577=EDGE_LOOP('',(#15759,#15760,#15761,#15762));
#3578=EDGE_LOOP('',(#15763,#15764,#15765,#15766));
#3579=EDGE_LOOP('',(#15767,#15768,#15769,#15770));
#3580=EDGE_LOOP('',(#15771,#15772,#15773,#15774));
#3581=EDGE_LOOP('',(#15775,#15776,#15777,#15778));
#3582=EDGE_LOOP('',(#15779,#15780,#15781,#15782));
#3583=EDGE_LOOP('',(#15783,#15784,#15785,#15786));
#3584=EDGE_LOOP('',(#15787,#15788,#15789,#15790,#15791));
#3585=EDGE_LOOP('',(#15792,#15793,#15794,#15795));
#3586=EDGE_LOOP('',(#15796,#15797,#15798,#15799));
#3587=EDGE_LOOP('',(#15800,#15801,#15802,#15803));
#3588=EDGE_LOOP('',(#15804,#15805,#15806,#15807));
#3589=EDGE_LOOP('',(#15808,#15809,#15810,#15811));
#3590=EDGE_LOOP('',(#15812,#15813,#15814,#15815));
#3591=EDGE_LOOP('',(#15816,#15817,#15818,#15819));
#3592=EDGE_LOOP('',(#15820,#15821,#15822,#15823));
#3593=EDGE_LOOP('',(#15824,#15825,#15826,#15827));
#3594=EDGE_LOOP('',(#15828,#15829,#15830,#15831));
#3595=EDGE_LOOP('',(#15832,#15833,#15834,#15835));
#3596=EDGE_LOOP('',(#15836,#15837,#15838,#15839));
#3597=EDGE_LOOP('',(#15840,#15841,#15842,#15843));
#3598=EDGE_LOOP('',(#15844,#15845,#15846,#15847));
#3599=EDGE_LOOP('',(#15848,#15849,#15850,#15851));
#3600=EDGE_LOOP('',(#15852,#15853,#15854,#15855));
#3601=EDGE_LOOP('',(#15856,#15857,#15858,#15859));
#3602=EDGE_LOOP('',(#15860,#15861,#15862,#15863));
#3603=EDGE_LOOP('',(#15864,#15865,#15866,#15867));
#3604=EDGE_LOOP('',(#15868,#15869,#15870,#15871));
#3605=EDGE_LOOP('',(#15872,#15873,#15874,#15875));
#3606=EDGE_LOOP('',(#15876,#15877,#15878,#15879));
#3607=EDGE_LOOP('',(#15880,#15881,#15882,#15883));
#3608=EDGE_LOOP('',(#15884,#15885,#15886,#15887));
#3609=EDGE_LOOP('',(#15888,#15889,#15890,#15891));
#3610=EDGE_LOOP('',(#15892,#15893,#15894,#15895));
#3611=EDGE_LOOP('',(#15896,#15897,#15898,#15899));
#3612=EDGE_LOOP('',(#15900,#15901,#15902,#15903));
#3613=EDGE_LOOP('',(#15904,#15905,#15906,#15907));
#3614=EDGE_LOOP('',(#15908,#15909,#15910,#15911));
#3615=EDGE_LOOP('',(#15912,#15913,#15914,#15915));
#3616=EDGE_LOOP('',(#15916,#15917,#15918,#15919));
#3617=EDGE_LOOP('',(#15920,#15921,#15922,#15923));
#3618=EDGE_LOOP('',(#15924,#15925,#15926,#15927));
#3619=EDGE_LOOP('',(#15928,#15929,#15930,#15931));
#3620=EDGE_LOOP('',(#15932,#15933,#15934,#15935));
#3621=EDGE_LOOP('',(#15936,#15937,#15938,#15939));
#3622=EDGE_LOOP('',(#15940,#15941,#15942,#15943));
#3623=EDGE_LOOP('',(#15944,#15945,#15946,#15947));
#3624=EDGE_LOOP('',(#15948,#15949,#15950,#15951));
#3625=EDGE_LOOP('',(#15952,#15953,#15954,#15955));
#3626=EDGE_LOOP('',(#15956,#15957,#15958,#15959));
#3627=EDGE_LOOP('',(#15960,#15961,#15962,#15963));
#3628=EDGE_LOOP('',(#15964,#15965,#15966,#15967));
#3629=EDGE_LOOP('',(#15968,#15969,#15970,#15971));
#3630=EDGE_LOOP('',(#15972,#15973,#15974,#15975));
#3631=EDGE_LOOP('',(#15976,#15977,#15978,#15979));
#3632=EDGE_LOOP('',(#15980,#15981,#15982,#15983));
#3633=EDGE_LOOP('',(#15984,#15985,#15986,#15987));
#3634=EDGE_LOOP('',(#15988,#15989,#15990,#15991));
#3635=EDGE_LOOP('',(#15992,#15993,#15994,#15995));
#3636=EDGE_LOOP('',(#15996,#15997,#15998,#15999));
#3637=EDGE_LOOP('',(#16000,#16001,#16002,#16003));
#3638=EDGE_LOOP('',(#16004,#16005,#16006,#16007));
#3639=EDGE_LOOP('',(#16008,#16009,#16010,#16011));
#3640=EDGE_LOOP('',(#16012,#16013,#16014,#16015));
#3641=EDGE_LOOP('',(#16016,#16017,#16018,#16019));
#3642=EDGE_LOOP('',(#16020,#16021,#16022,#16023));
#3643=EDGE_LOOP('',(#16024,#16025,#16026,#16027));
#3644=EDGE_LOOP('',(#16028,#16029,#16030,#16031));
#3645=EDGE_LOOP('',(#16032,#16033,#16034,#16035));
#3646=EDGE_LOOP('',(#16036,#16037,#16038,#16039));
#3647=EDGE_LOOP('',(#16040,#16041,#16042,#16043));
#3648=EDGE_LOOP('',(#16044,#16045,#16046,#16047));
#3649=EDGE_LOOP('',(#16048,#16049,#16050,#16051));
#3650=EDGE_LOOP('',(#16052,#16053,#16054,#16055));
#3651=EDGE_LOOP('',(#16056,#16057,#16058,#16059));
#3652=EDGE_LOOP('',(#16060,#16061,#16062,#16063));
#3653=EDGE_LOOP('',(#16064,#16065,#16066,#16067));
#3654=EDGE_LOOP('',(#16068,#16069,#16070,#16071));
#3655=EDGE_LOOP('',(#16072,#16073,#16074,#16075));
#3656=EDGE_LOOP('',(#16076,#16077,#16078,#16079));
#3657=EDGE_LOOP('',(#16080,#16081,#16082,#16083));
#3658=EDGE_LOOP('',(#16084,#16085,#16086,#16087));
#3659=EDGE_LOOP('',(#16088,#16089,#16090,#16091));
#3660=EDGE_LOOP('',(#16092,#16093,#16094,#16095));
#3661=EDGE_LOOP('',(#16096,#16097,#16098,#16099));
#3662=EDGE_LOOP('',(#16100,#16101,#16102,#16103));
#3663=EDGE_LOOP('',(#16104,#16105,#16106,#16107,#16108));
#3664=EDGE_LOOP('',(#16109,#16110,#16111,#16112));
#3665=EDGE_LOOP('',(#16113,#16114,#16115,#16116));
#3666=EDGE_LOOP('',(#16117,#16118,#16119,#16120));
#3667=EDGE_LOOP('',(#16121,#16122,#16123,#16124));
#3668=EDGE_LOOP('',(#16125,#16126,#16127,#16128));
#3669=EDGE_LOOP('',(#16129,#16130,#16131,#16132));
#3670=EDGE_LOOP('',(#16133,#16134,#16135,#16136));
#3671=EDGE_LOOP('',(#16137,#16138,#16139,#16140));
#3672=EDGE_LOOP('',(#16141,#16142,#16143,#16144));
#3673=EDGE_LOOP('',(#16145,#16146,#16147,#16148));
#3674=EDGE_LOOP('',(#16149,#16150,#16151,#16152));
#3675=EDGE_LOOP('',(#16153,#16154,#16155,#16156));
#3676=EDGE_LOOP('',(#16157,#16158,#16159,#16160));
#3677=EDGE_LOOP('',(#16161,#16162,#16163,#16164));
#3678=EDGE_LOOP('',(#16165,#16166,#16167,#16168));
#3679=EDGE_LOOP('',(#16169,#16170,#16171,#16172));
#3680=EDGE_LOOP('',(#16173,#16174,#16175,#16176));
#3681=EDGE_LOOP('',(#16177,#16178,#16179,#16180));
#3682=EDGE_LOOP('',(#16181,#16182,#16183,#16184));
#3683=EDGE_LOOP('',(#16185,#16186,#16187,#16188));
#3684=EDGE_LOOP('',(#16189,#16190,#16191,#16192));
#3685=EDGE_LOOP('',(#16193,#16194,#16195,#16196));
#3686=EDGE_LOOP('',(#16197,#16198,#16199,#16200));
#3687=EDGE_LOOP('',(#16201,#16202,#16203,#16204));
#3688=EDGE_LOOP('',(#16205,#16206,#16207,#16208));
#3689=EDGE_LOOP('',(#16209,#16210,#16211,#16212));
#3690=EDGE_LOOP('',(#16213,#16214,#16215,#16216));
#3691=EDGE_LOOP('',(#16217,#16218,#16219,#16220));
#3692=EDGE_LOOP('',(#16221,#16222,#16223,#16224));
#3693=EDGE_LOOP('',(#16225,#16226,#16227,#16228));
#3694=EDGE_LOOP('',(#16229,#16230,#16231,#16232));
#3695=EDGE_LOOP('',(#16233,#16234,#16235,#16236));
#3696=EDGE_LOOP('',(#16237,#16238,#16239,#16240));
#3697=EDGE_LOOP('',(#16241,#16242,#16243,#16244));
#3698=LINE('',#24606,#4642);
#3699=LINE('',#24609,#4643);
#3700=LINE('',#24615,#4644);
#3701=LINE('',#24618,#4645);
#3702=LINE('',#24621,#4646);
#3703=LINE('',#24623,#4647);
#3704=LINE('',#24625,#4648);
#3705=LINE('',#24627,#4649);
#3706=LINE('',#24628,#4650);
#3707=LINE('',#24629,#4651);
#3708=LINE('',#24632,#4652);
#3709=LINE('',#24633,#4653);
#3710=LINE('',#24635,#4654);
#3711=LINE('',#24637,#4655);
#3712=LINE('',#24639,#4656);
#3713=LINE('',#24640,#4657);
#3714=LINE('',#24656,#4658);
#3715=LINE('',#24659,#4659);
#3716=LINE('',#24665,#4660);
#3717=LINE('',#24668,#4661);
#3718=LINE('',#24674,#4662);
#3719=LINE('',#24677,#4663);
#3720=LINE('',#24679,#4664);
#3721=LINE('',#24680,#4665);
#3722=LINE('',#24682,#4666);
#3723=LINE('',#24684,#4667);
#3724=LINE('',#24685,#4668);
#3725=LINE('',#24687,#4669);
#3726=LINE('',#24689,#4670);
#3727=LINE('',#24691,#4671);
#3728=LINE('',#24692,#4672);
#3729=LINE('',#24693,#4673);
#3730=LINE('',#24704,#4674);
#3731=LINE('',#24706,#4675);
#3732=LINE('',#24708,#4676);
#3733=LINE('',#24709,#4677);
#3734=LINE('',#24713,#4678);
#3735=LINE('',#24714,#4679);
#3736=LINE('',#24716,#4680);
#3737=LINE('',#24718,#4681);
#3738=LINE('',#24720,#4682);
#3739=LINE('',#24722,#4683);
#3740=LINE('',#24723,#4684);
#3741=LINE('',#24726,#4685);
#3742=LINE('',#24728,#4686);
#3743=LINE('',#24730,#4687);
#3744=LINE('',#24732,#4688);
#3745=LINE('',#24734,#4689);
#3746=LINE('',#24736,#4690);
#3747=LINE('',#24737,#4691);
#3748=LINE('',#24754,#4692);
#3749=LINE('',#24756,#4693);
#3750=LINE('',#24758,#4694);
#3751=LINE('',#24759,#4695);
#3752=LINE('',#24763,#4696);
#3753=LINE('',#24764,#4697);
#3754=LINE('',#24766,#4698);
#3755=LINE('',#24768,#4699);
#3756=LINE('',#24770,#4700);
#3757=LINE('',#24772,#4701);
#3758=LINE('',#24773,#4702);
#3759=LINE('',#24776,#4703);
#3760=LINE('',#24778,#4704);
#3761=LINE('',#24780,#4705);
#3762=LINE('',#24782,#4706);
#3763=LINE('',#24784,#4707);
#3764=LINE('',#24786,#4708);
#3765=LINE('',#24787,#4709);
#3766=LINE('',#24807,#4710);
#3767=LINE('',#24810,#4711);
#3768=LINE('',#24815,#4712);
#3769=LINE('',#24818,#4713);
#3770=LINE('',#24819,#4714);
#3771=LINE('',#24821,#4715);
#3772=LINE('',#24822,#4716);
#3773=LINE('',#24823,#4717);
#3774=LINE('',#24833,#4718);
#3775=LINE('',#24836,#4719);
#3776=LINE('',#24842,#4720);
#3777=LINE('',#24845,#4721);
#3778=LINE('',#24847,#4722);
#3779=LINE('',#24849,#4723);
#3780=LINE('',#24850,#4724);
#3781=LINE('',#24851,#4725);
#3782=LINE('',#24857,#4726);
#3783=LINE('',#24859,#4727);
#3784=LINE('',#24861,#4728);
#3785=LINE('',#24862,#4729);
#3786=LINE('',#24866,#4730);
#3787=LINE('',#24868,#4731);
#3788=LINE('',#24870,#4732);
#3789=LINE('',#24872,#4733);
#3790=LINE('',#24874,#4734);
#3791=LINE('',#24875,#4735);
#3792=LINE('',#24876,#4736);
#3793=LINE('',#24880,#4737);
#3794=LINE('',#24881,#4738);
#3795=LINE('',#24882,#4739);
#3796=LINE('',#24885,#4740);
#3797=LINE('',#24887,#4741);
#3798=LINE('',#24889,#4742);
#3799=LINE('',#24891,#4743);
#3800=LINE('',#24892,#4744);
#3801=LINE('',#24893,#4745);
#3802=LINE('',#24907,#4746);
#3803=LINE('',#24911,#4747);
#3804=LINE('',#24950,#4748);
#3805=LINE('',#24958,#4749);
#3806=LINE('',#24963,#4750);
#3807=LINE('',#24967,#4751);
#3808=LINE('',#24975,#4752);
#3809=LINE('',#24985,#4753);
#3810=LINE('',#24996,#4754);
#3811=LINE('',#25026,#4755);
#3812=LINE('',#25056,#4756);
#3813=LINE('',#25086,#4757);
#3814=LINE('',#25116,#4758);
#3815=LINE('',#25146,#4759);
#3816=LINE('',#25176,#4760);
#3817=LINE('',#25206,#4761);
#3818=LINE('',#25236,#4762);
#3819=LINE('',#25266,#4763);
#3820=LINE('',#25296,#4764);
#3821=LINE('',#25326,#4765);
#3822=LINE('',#25356,#4766);
#3823=LINE('',#25386,#4767);
#3824=LINE('',#25416,#4768);
#3825=LINE('',#25446,#4769);
#3826=LINE('',#25476,#4770);
#3827=LINE('',#25506,#4771);
#3828=LINE('',#25536,#4772);
#3829=LINE('',#25566,#4773);
#3830=LINE('',#25596,#4774);
#3831=LINE('',#25626,#4775);
#3832=LINE('',#25656,#4776);
#3833=LINE('',#25686,#4777);
#3834=LINE('',#25703,#4778);
#3835=LINE('',#25745,#4779);
#3836=LINE('',#25783,#4780);
#3837=LINE('',#25826,#4781);
#3838=LINE('',#25902,#4782);
#3839=LINE('',#25978,#4783);
#3840=LINE('',#26054,#4784);
#3841=LINE('',#26130,#4785);
#3842=LINE('',#26208,#4786);
#3843=LINE('',#26286,#4787);
#3844=LINE('',#26362,#4788);
#3845=LINE('',#26438,#4789);
#3846=LINE('',#26514,#4790);
#3847=LINE('',#26590,#4791);
#3848=LINE('',#26670,#4792);
#3849=LINE('',#26746,#4793);
#3850=LINE('',#26822,#4794);
#3851=LINE('',#26898,#4795);
#3852=LINE('',#26974,#4796);
#3853=LINE('',#27050,#4797);
#3854=LINE('',#27130,#4798);
#3855=LINE('',#27206,#4799);
#3856=LINE('',#27282,#4800);
#3857=LINE('',#27358,#4801);
#3858=LINE('',#27434,#4802);
#3859=LINE('',#27510,#4803);
#3860=LINE('',#27540,#4804);
#3861=LINE('',#27546,#4805);
#3862=LINE('',#27587,#4806);
#3863=LINE('',#27637,#4807);
#3864=LINE('',#27815,#4808);
#3865=LINE('',#28001,#4809);
#3866=LINE('',#28006,#4810);
#3867=LINE('',#28226,#4811);
#3868=LINE('',#28227,#4812);
#3869=LINE('',#28229,#4813);
#3870=LINE('',#28338,#4814);
#3871=LINE('',#28341,#4815);
#3872=LINE('',#28342,#4816);
#3873=LINE('',#29891,#4817);
#3874=LINE('',#29897,#4818);
#3875=LINE('',#29907,#4819);
#3876=LINE('',#29913,#4820);
#3877=LINE('',#29934,#4821);
#3878=LINE('',#29937,#4822);
#3879=LINE('',#29949,#4823);
#3880=LINE('',#29953,#4824);
#3881=LINE('',#29959,#4825);
#3882=LINE('',#29963,#4826);
#3883=LINE('',#29973,#4827);
#3884=LINE('',#29983,#4828);
#3885=LINE('',#30000,#4829);
#3886=LINE('',#30025,#4830);
#3887=LINE('',#30446,#4831);
#3888=LINE('',#30628,#4832);
#3889=LINE('',#30641,#4833);
#3890=LINE('',#30654,#4834);
#3891=LINE('',#30767,#4835);
#3892=LINE('',#31044,#4836);
#3893=LINE('',#31240,#4837);
#3894=LINE('',#31246,#4838);
#3895=LINE('',#31251,#4839);
#3896=LINE('',#31253,#4840);
#3897=LINE('',#32014,#4841);
#3898=LINE('',#32022,#4842);
#3899=LINE('',#32026,#4843);
#3900=LINE('',#32030,#4844);
#3901=LINE('',#32136,#4845);
#3902=LINE('',#32160,#4846);
#3903=LINE('',#32277,#4847);
#3904=LINE('',#32490,#4848);
#3905=LINE('',#32495,#4849);
#3906=LINE('',#32547,#4850);
#3907=LINE('',#32678,#4851);
#3908=LINE('',#32988,#4852);
#3909=LINE('',#32996,#4853);
#3910=LINE('',#33000,#4854);
#3911=LINE('',#33004,#4855);
#3912=LINE('',#33022,#4856);
#3913=LINE('',#33029,#4857);
#3914=LINE('',#33032,#4858);
#3915=LINE('',#33039,#4859);
#3916=LINE('',#33044,#4860);
#3917=LINE('',#33048,#4861);
#3918=LINE('',#33069,#4862);
#3919=LINE('',#33072,#4863);
#3920=LINE('',#33095,#4864);
#3921=LINE('',#33098,#4865);
#3922=LINE('',#33112,#4866);
#3923=LINE('',#33115,#4867);
#3924=LINE('',#33138,#4868);
#3925=LINE('',#33140,#4869);
#3926=LINE('',#33143,#4870);
#3927=LINE('',#33147,#4871);
#3928=LINE('',#33151,#4872);
#3929=LINE('',#33154,#4873);
#3930=LINE('',#33159,#4874);
#3931=LINE('',#33165,#4875);
#3932=LINE('',#33172,#4876);
#3933=LINE('',#33175,#4877);
#3934=LINE('',#33180,#4878);
#3935=LINE('',#33189,#4879);
#3936=LINE('',#33196,#4880);
#3937=LINE('',#33199,#4881);
#3938=LINE('',#33262,#4882);
#3939=LINE('',#33263,#4883);
#3940=LINE('',#33281,#4884);
#3941=LINE('',#33284,#4885);
#3942=LINE('',#33287,#4886);
#3943=LINE('',#33291,#4887);
#3944=LINE('',#33364,#4888);
#3945=LINE('',#33372,#4889);
#3946=LINE('',#33380,#4890);
#3947=LINE('',#33386,#4891);
#3948=LINE('',#33407,#4892);
#3949=LINE('',#33415,#4893);
#3950=LINE('',#33421,#4894);
#3951=LINE('',#33427,#4895);
#3952=LINE('',#33444,#4896);
#3953=LINE('',#33479,#4897);
#3954=LINE('',#33481,#4898);
#3955=LINE('',#33483,#4899);
#3956=LINE('',#33484,#4900);
#3957=LINE('',#33485,#4901);
#3958=LINE('',#33487,#4902);
#3959=LINE('',#33489,#4903);
#3960=LINE('',#33493,#4904);
#3961=LINE('',#33495,#4905);
#3962=LINE('',#33497,#4906);
#3963=LINE('',#33498,#4907);
#3964=LINE('',#33502,#4908);
#3965=LINE('',#33504,#4909);
#3966=LINE('',#33506,#4910);
#3967=LINE('',#33507,#4911);
#3968=LINE('',#33510,#4912);
#3969=LINE('',#33514,#4913);
#3970=LINE('',#33516,#4914);
#3971=LINE('',#33517,#4915);
#3972=LINE('',#33519,#4916);
#3973=LINE('',#33521,#4917);
#3974=LINE('',#33523,#4918);
#3975=LINE('',#33525,#4919);
#3976=LINE('',#33527,#4920);
#3977=LINE('',#33529,#4921);
#3978=LINE('',#33531,#4922);
#3979=LINE('',#33534,#4923);
#3980=LINE('',#33537,#4924);
#3981=LINE('',#33539,#4925);
#3982=LINE('',#33540,#4926);
#3983=LINE('',#33543,#4927);
#3984=LINE('',#33545,#4928);
#3985=LINE('',#33549,#4929);
#3986=LINE('',#33551,#4930);
#3987=LINE('',#33552,#4931);
#3988=LINE('',#33554,#4932);
#3989=LINE('',#33556,#4933);
#3990=LINE('',#33558,#4934);
#3991=LINE('',#33560,#4935);
#3992=LINE('',#33562,#4936);
#3993=LINE('',#33564,#4937);
#3994=LINE('',#33565,#4938);
#3995=LINE('',#33567,#4939);
#3996=LINE('',#33569,#4940);
#3997=LINE('',#33571,#4941);
#3998=LINE('',#33576,#4942);
#3999=LINE('',#33578,#4943);
#4000=LINE('',#33580,#4944);
#4001=LINE('',#33581,#4945);
#4002=LINE('',#33585,#4946);
#4003=LINE('',#33587,#4947);
#4004=LINE('',#33589,#4948);
#4005=LINE('',#33591,#4949);
#4006=LINE('',#33593,#4950);
#4007=LINE('',#33594,#4951);
#4008=LINE('',#33595,#4952);
#4009=LINE('',#33599,#4953);
#4010=LINE('',#33601,#4954);
#4011=LINE('',#33603,#4955);
#4012=LINE('',#33605,#4956);
#4013=LINE('',#33609,#4957);
#4014=LINE('',#33610,#4958);
#4015=LINE('',#33614,#4959);
#4016=LINE('',#33616,#4960);
#4017=LINE('',#33618,#4961);
#4018=LINE('',#33620,#4962);
#4019=LINE('',#33624,#4963);
#4020=LINE('',#33626,#4964);
#4021=LINE('',#33628,#4965);
#4022=LINE('',#33629,#4966);
#4023=LINE('',#33633,#4967);
#4024=LINE('',#33637,#4968);
#4025=LINE('',#33651,#4969);
#4026=LINE('',#33663,#4970);
#4027=LINE('',#33675,#4971);
#4028=LINE('',#33677,#4972);
#4029=LINE('',#33680,#4973);
#4030=LINE('',#33682,#4974);
#4031=LINE('',#33694,#4975);
#4032=LINE('',#33696,#4976);
#4033=LINE('',#33700,#4977);
#4034=LINE('',#33701,#4978);
#4035=LINE('',#33704,#4979);
#4036=LINE('',#33705,#4980);
#4037=LINE('',#33708,#4981);
#4038=LINE('',#33710,#4982);
#4039=LINE('',#33711,#4983);
#4040=LINE('',#33714,#4984);
#4041=LINE('',#33715,#4985);
#4042=LINE('',#33721,#4986);
#4043=LINE('',#33722,#4987);
#4044=LINE('',#33727,#4988);
#4045=LINE('',#33728,#4989);
#4046=LINE('',#33729,#4990);
#4047=LINE('',#33814,#4991);
#4048=LINE('',#33821,#4992);
#4049=LINE('',#33830,#4993);
#4050=LINE('',#33837,#4994);
#4051=LINE('',#33843,#4995);
#4052=LINE('',#33849,#4996);
#4053=LINE('',#33855,#4997);
#4054=LINE('',#33859,#4998);
#4055=LINE('',#33861,#4999);
#4056=LINE('',#33862,#5000);
#4057=LINE('',#33866,#5001);
#4058=LINE('',#33870,#5002);
#4059=LINE('',#33874,#5003);
#4060=LINE('',#33876,#5004);
#4061=LINE('',#33877,#5005);
#4062=LINE('',#33879,#5006);
#4063=LINE('',#33880,#5007);
#4064=LINE('',#33884,#5008);
#4065=LINE('',#33886,#5009);
#4066=LINE('',#33888,#5010);
#4067=LINE('',#33891,#5011);
#4068=LINE('',#33893,#5012);
#4069=LINE('',#33894,#5013);
#4070=LINE('',#33898,#5014);
#4071=LINE('',#33899,#5015);
#4072=LINE('',#33901,#5016);
#4073=LINE('',#33902,#5017);
#4074=LINE('',#33905,#5018);
#4075=LINE('',#33909,#5019);
#4076=LINE('',#33910,#5020);
#4077=LINE('',#33913,#5021);
#4078=LINE('',#33915,#5022);
#4079=LINE('',#33916,#5023);
#4080=LINE('',#33918,#5024);
#4081=LINE('',#33920,#5025);
#4082=LINE('',#33929,#5026);
#4083=LINE('',#33948,#5027);
#4084=LINE('',#33956,#5028);
#4085=LINE('',#33961,#5029);
#4086=LINE('',#33967,#5030);
#4087=LINE('',#33974,#5031);
#4088=LINE('',#33979,#5032);
#4089=LINE('',#33985,#5033);
#4090=LINE('',#33992,#5034);
#4091=LINE('',#33997,#5035);
#4092=LINE('',#34003,#5036);
#4093=LINE('',#34010,#5037);
#4094=LINE('',#34015,#5038);
#4095=LINE('',#34021,#5039);
#4096=LINE('',#34028,#5040);
#4097=LINE('',#34033,#5041);
#4098=LINE('',#34039,#5042);
#4099=LINE('',#34046,#5043);
#4100=LINE('',#34051,#5044);
#4101=LINE('',#34057,#5045);
#4102=LINE('',#34064,#5046);
#4103=LINE('',#34069,#5047);
#4104=LINE('',#34075,#5048);
#4105=LINE('',#34082,#5049);
#4106=LINE('',#34087,#5050);
#4107=LINE('',#34093,#5051);
#4108=LINE('',#34100,#5052);
#4109=LINE('',#34105,#5053);
#4110=LINE('',#34111,#5054);
#4111=LINE('',#34118,#5055);
#4112=LINE('',#34123,#5056);
#4113=LINE('',#34129,#5057);
#4114=LINE('',#34136,#5058);
#4115=LINE('',#34141,#5059);
#4116=LINE('',#34147,#5060);
#4117=LINE('',#34154,#5061);
#4118=LINE('',#34159,#5062);
#4119=LINE('',#34165,#5063);
#4120=LINE('',#34172,#5064);
#4121=LINE('',#34177,#5065);
#4122=LINE('',#34183,#5066);
#4123=LINE('',#34190,#5067);
#4124=LINE('',#34195,#5068);
#4125=LINE('',#34201,#5069);
#4126=LINE('',#34208,#5070);
#4127=LINE('',#34213,#5071);
#4128=LINE('',#34607,#5072);
#4129=LINE('',#35385,#5073);
#4130=LINE('',#35771,#5074);
#4131=LINE('',#35773,#5075);
#4132=LINE('',#35774,#5076);
#4133=LINE('',#35776,#5077);
#4134=LINE('',#35777,#5078);
#4135=LINE('',#35779,#5079);
#4136=LINE('',#35780,#5080);
#4137=LINE('',#35782,#5081);
#4138=LINE('',#35783,#5082);
#4139=LINE('',#35785,#5083);
#4140=LINE('',#35786,#5084);
#4141=LINE('',#35788,#5085);
#4142=LINE('',#35789,#5086);
#4143=LINE('',#35791,#5087);
#4144=LINE('',#35792,#5088);
#4145=LINE('',#35794,#5089);
#4146=LINE('',#35795,#5090);
#4147=LINE('',#35797,#5091);
#4148=LINE('',#35798,#5092);
#4149=LINE('',#35800,#5093);
#4150=LINE('',#35801,#5094);
#4151=LINE('',#35803,#5095);
#4152=LINE('',#35804,#5096);
#4153=LINE('',#35806,#5097);
#4154=LINE('',#35807,#5098);
#4155=LINE('',#35809,#5099);
#4156=LINE('',#35810,#5100);
#4157=LINE('',#35812,#5101);
#4158=LINE('',#35813,#5102);
#4159=LINE('',#35815,#5103);
#4160=LINE('',#35816,#5104);
#4161=LINE('',#35818,#5105);
#4162=LINE('',#35819,#5106);
#4163=LINE('',#35821,#5107);
#4164=LINE('',#35822,#5108);
#4165=LINE('',#35824,#5109);
#4166=LINE('',#35825,#5110);
#4167=LINE('',#35827,#5111);
#4168=LINE('',#35828,#5112);
#4169=LINE('',#35830,#5113);
#4170=LINE('',#35831,#5114);
#4171=LINE('',#35833,#5115);
#4172=LINE('',#35834,#5116);
#4173=LINE('',#35836,#5117);
#4174=LINE('',#35837,#5118);
#4175=LINE('',#35839,#5119);
#4176=LINE('',#35840,#5120);
#4177=LINE('',#35842,#5121);
#4178=LINE('',#35843,#5122);
#4179=LINE('',#35845,#5123);
#4180=LINE('',#35846,#5124);
#4181=LINE('',#35848,#5125);
#4182=LINE('',#35849,#5126);
#4183=LINE('',#35851,#5127);
#4184=LINE('',#35852,#5128);
#4185=LINE('',#35854,#5129);
#4186=LINE('',#35855,#5130);
#4187=LINE('',#35857,#5131);
#4188=LINE('',#35858,#5132);
#4189=LINE('',#35860,#5133);
#4190=LINE('',#35861,#5134);
#4191=LINE('',#35863,#5135);
#4192=LINE('',#35864,#5136);
#4193=LINE('',#35866,#5137);
#4194=LINE('',#35867,#5138);
#4195=LINE('',#35869,#5139);
#4196=LINE('',#35870,#5140);
#4197=LINE('',#35872,#5141);
#4198=LINE('',#35873,#5142);
#4199=LINE('',#35875,#5143);
#4200=LINE('',#35876,#5144);
#4201=LINE('',#35878,#5145);
#4202=LINE('',#35879,#5146);
#4203=LINE('',#35881,#5147);
#4204=LINE('',#35882,#5148);
#4205=LINE('',#35884,#5149);
#4206=LINE('',#35885,#5150);
#4207=LINE('',#35887,#5151);
#4208=LINE('',#35888,#5152);
#4209=LINE('',#35890,#5153);
#4210=LINE('',#35891,#5154);
#4211=LINE('',#35893,#5155);
#4212=LINE('',#35894,#5156);
#4213=LINE('',#35896,#5157);
#4214=LINE('',#35897,#5158);
#4215=LINE('',#35899,#5159);
#4216=LINE('',#35900,#5160);
#4217=LINE('',#35902,#5161);
#4218=LINE('',#35903,#5162);
#4219=LINE('',#35905,#5163);
#4220=LINE('',#35906,#5164);
#4221=LINE('',#35908,#5165);
#4222=LINE('',#35909,#5166);
#4223=LINE('',#35911,#5167);
#4224=LINE('',#35912,#5168);
#4225=LINE('',#35914,#5169);
#4226=LINE('',#35915,#5170);
#4227=LINE('',#35917,#5171);
#4228=LINE('',#35918,#5172);
#4229=LINE('',#35920,#5173);
#4230=LINE('',#35921,#5174);
#4231=LINE('',#35923,#5175);
#4232=LINE('',#35924,#5176);
#4233=LINE('',#35926,#5177);
#4234=LINE('',#35927,#5178);
#4235=LINE('',#35929,#5179);
#4236=LINE('',#35930,#5180);
#4237=LINE('',#35932,#5181);
#4238=LINE('',#35933,#5182);
#4239=LINE('',#35935,#5183);
#4240=LINE('',#35936,#5184);
#4241=LINE('',#35938,#5185);
#4242=LINE('',#35939,#5186);
#4243=LINE('',#35941,#5187);
#4244=LINE('',#35942,#5188);
#4245=LINE('',#35944,#5189);
#4246=LINE('',#35945,#5190);
#4247=LINE('',#35947,#5191);
#4248=LINE('',#35948,#5192);
#4249=LINE('',#35950,#5193);
#4250=LINE('',#35951,#5194);
#4251=LINE('',#35953,#5195);
#4252=LINE('',#35954,#5196);
#4253=LINE('',#35956,#5197);
#4254=LINE('',#35957,#5198);
#4255=LINE('',#35959,#5199);
#4256=LINE('',#35960,#5200);
#4257=LINE('',#35962,#5201);
#4258=LINE('',#35963,#5202);
#4259=LINE('',#35965,#5203);
#4260=LINE('',#35966,#5204);
#4261=LINE('',#35968,#5205);
#4262=LINE('',#35969,#5206);
#4263=LINE('',#35971,#5207);
#4264=LINE('',#35972,#5208);
#4265=LINE('',#35974,#5209);
#4266=LINE('',#35975,#5210);
#4267=LINE('',#35977,#5211);
#4268=LINE('',#35978,#5212);
#4269=LINE('',#35980,#5213);
#4270=LINE('',#35981,#5214);
#4271=LINE('',#35983,#5215);
#4272=LINE('',#35984,#5216);
#4273=LINE('',#35986,#5217);
#4274=LINE('',#35987,#5218);
#4275=LINE('',#35989,#5219);
#4276=LINE('',#35990,#5220);
#4277=LINE('',#35992,#5221);
#4278=LINE('',#35993,#5222);
#4279=LINE('',#35995,#5223);
#4280=LINE('',#35996,#5224);
#4281=LINE('',#35998,#5225);
#4282=LINE('',#35999,#5226);
#4283=LINE('',#36002,#5227);
#4284=LINE('',#36003,#5228);
#4285=LINE('',#36007,#5229);
#4286=LINE('',#36010,#5230);
#4287=LINE('',#36013,#5231);
#4288=LINE('',#36016,#5232);
#4289=LINE('',#36019,#5233);
#4290=LINE('',#36022,#5234);
#4291=LINE('',#36025,#5235);
#4292=LINE('',#36028,#5236);
#4293=LINE('',#36031,#5237);
#4294=LINE('',#36034,#5238);
#4295=LINE('',#36037,#5239);
#4296=LINE('',#36040,#5240);
#4297=LINE('',#36043,#5241);
#4298=LINE('',#36046,#5242);
#4299=LINE('',#36049,#5243);
#4300=LINE('',#36052,#5244);
#4301=LINE('',#36055,#5245);
#4302=LINE('',#36058,#5246);
#4303=LINE('',#36061,#5247);
#4304=LINE('',#36064,#5248);
#4305=LINE('',#36067,#5249);
#4306=LINE('',#36070,#5250);
#4307=LINE('',#36073,#5251);
#4308=LINE('',#36076,#5252);
#4309=LINE('',#36079,#5253);
#4310=LINE('',#36082,#5254);
#4311=LINE('',#36085,#5255);
#4312=LINE('',#36088,#5256);
#4313=LINE('',#36091,#5257);
#4314=LINE('',#36094,#5258);
#4315=LINE('',#36097,#5259);
#4316=LINE('',#36100,#5260);
#4317=LINE('',#36103,#5261);
#4318=LINE('',#36106,#5262);
#4319=LINE('',#36109,#5263);
#4320=LINE('',#36112,#5264);
#4321=LINE('',#36115,#5265);
#4322=LINE('',#36118,#5266);
#4323=LINE('',#36121,#5267);
#4324=LINE('',#36124,#5268);
#4325=LINE('',#36127,#5269);
#4326=LINE('',#36130,#5270);
#4327=LINE('',#36133,#5271);
#4328=LINE('',#36136,#5272);
#4329=LINE('',#36139,#5273);
#4330=LINE('',#36142,#5274);
#4331=LINE('',#36145,#5275);
#4332=LINE('',#36148,#5276);
#4333=LINE('',#36151,#5277);
#4334=LINE('',#36154,#5278);
#4335=LINE('',#36157,#5279);
#4336=LINE('',#36160,#5280);
#4337=LINE('',#36163,#5281);
#4338=LINE('',#36166,#5282);
#4339=LINE('',#36169,#5283);
#4340=LINE('',#36172,#5284);
#4341=LINE('',#36175,#5285);
#4342=LINE('',#36178,#5286);
#4343=LINE('',#36181,#5287);
#4344=LINE('',#36184,#5288);
#4345=LINE('',#36187,#5289);
#4346=LINE('',#36190,#5290);
#4347=LINE('',#36193,#5291);
#4348=LINE('',#36196,#5292);
#4349=LINE('',#36199,#5293);
#4350=LINE('',#36202,#5294);
#4351=LINE('',#36205,#5295);
#4352=LINE('',#36208,#5296);
#4353=LINE('',#36211,#5297);
#4354=LINE('',#36214,#5298);
#4355=LINE('',#36217,#5299);
#4356=LINE('',#36220,#5300);
#4357=LINE('',#36223,#5301);
#4358=LINE('',#36226,#5302);
#4359=LINE('',#36229,#5303);
#4360=LINE('',#36232,#5304);
#4361=LINE('',#36235,#5305);
#4362=LINE('',#36300,#5306);
#4363=LINE('',#36305,#5307);
#4364=LINE('',#36308,#5308);
#4365=LINE('',#36311,#5309);
#4366=LINE('',#36314,#5310);
#4367=LINE('',#36316,#5311);
#4368=LINE('',#36330,#5312);
#4369=LINE('',#36338,#5313);
#4370=LINE('',#36343,#5314);
#4371=LINE('',#36349,#5315);
#4372=LINE('',#36356,#5316);
#4373=LINE('',#36361,#5317);
#4374=LINE('',#36367,#5318);
#4375=LINE('',#36374,#5319);
#4376=LINE('',#36379,#5320);
#4377=LINE('',#36385,#5321);
#4378=LINE('',#36392,#5322);
#4379=LINE('',#36397,#5323);
#4380=LINE('',#36403,#5324);
#4381=LINE('',#36410,#5325);
#4382=LINE('',#36415,#5326);
#4383=LINE('',#36421,#5327);
#4384=LINE('',#36428,#5328);
#4385=LINE('',#36433,#5329);
#4386=LINE('',#36439,#5330);
#4387=LINE('',#36446,#5331);
#4388=LINE('',#36451,#5332);
#4389=LINE('',#36457,#5333);
#4390=LINE('',#36464,#5334);
#4391=LINE('',#36469,#5335);
#4392=LINE('',#36475,#5336);
#4393=LINE('',#36482,#5337);
#4394=LINE('',#36487,#5338);
#4395=LINE('',#36493,#5339);
#4396=LINE('',#36500,#5340);
#4397=LINE('',#36505,#5341);
#4398=LINE('',#36511,#5342);
#4399=LINE('',#36518,#5343);
#4400=LINE('',#36523,#5344);
#4401=LINE('',#36529,#5345);
#4402=LINE('',#36536,#5346);
#4403=LINE('',#36541,#5347);
#4404=LINE('',#36547,#5348);
#4405=LINE('',#36554,#5349);
#4406=LINE('',#36559,#5350);
#4407=LINE('',#36562,#5351);
#4408=LINE('',#36957,#5352);
#4409=LINE('',#37735,#5353);
#4410=LINE('',#38123,#5354);
#4411=LINE('',#38125,#5355);
#4412=LINE('',#38126,#5356);
#4413=LINE('',#38128,#5357);
#4414=LINE('',#38129,#5358);
#4415=LINE('',#38131,#5359);
#4416=LINE('',#38132,#5360);
#4417=LINE('',#38134,#5361);
#4418=LINE('',#38135,#5362);
#4419=LINE('',#38137,#5363);
#4420=LINE('',#38138,#5364);
#4421=LINE('',#38140,#5365);
#4422=LINE('',#38141,#5366);
#4423=LINE('',#38143,#5367);
#4424=LINE('',#38144,#5368);
#4425=LINE('',#38146,#5369);
#4426=LINE('',#38147,#5370);
#4427=LINE('',#38149,#5371);
#4428=LINE('',#38150,#5372);
#4429=LINE('',#38152,#5373);
#4430=LINE('',#38153,#5374);
#4431=LINE('',#38155,#5375);
#4432=LINE('',#38156,#5376);
#4433=LINE('',#38158,#5377);
#4434=LINE('',#38159,#5378);
#4435=LINE('',#38161,#5379);
#4436=LINE('',#38162,#5380);
#4437=LINE('',#38164,#5381);
#4438=LINE('',#38165,#5382);
#4439=LINE('',#38167,#5383);
#4440=LINE('',#38168,#5384);
#4441=LINE('',#38170,#5385);
#4442=LINE('',#38171,#5386);
#4443=LINE('',#38173,#5387);
#4444=LINE('',#38174,#5388);
#4445=LINE('',#38176,#5389);
#4446=LINE('',#38177,#5390);
#4447=LINE('',#38179,#5391);
#4448=LINE('',#38180,#5392);
#4449=LINE('',#38182,#5393);
#4450=LINE('',#38183,#5394);
#4451=LINE('',#38185,#5395);
#4452=LINE('',#38186,#5396);
#4453=LINE('',#38188,#5397);
#4454=LINE('',#38189,#5398);
#4455=LINE('',#38191,#5399);
#4456=LINE('',#38192,#5400);
#4457=LINE('',#38194,#5401);
#4458=LINE('',#38195,#5402);
#4459=LINE('',#38197,#5403);
#4460=LINE('',#38198,#5404);
#4461=LINE('',#38200,#5405);
#4462=LINE('',#38201,#5406);
#4463=LINE('',#38203,#5407);
#4464=LINE('',#38204,#5408);
#4465=LINE('',#38206,#5409);
#4466=LINE('',#38207,#5410);
#4467=LINE('',#38209,#5411);
#4468=LINE('',#38210,#5412);
#4469=LINE('',#38212,#5413);
#4470=LINE('',#38213,#5414);
#4471=LINE('',#38215,#5415);
#4472=LINE('',#38216,#5416);
#4473=LINE('',#38218,#5417);
#4474=LINE('',#38219,#5418);
#4475=LINE('',#38221,#5419);
#4476=LINE('',#38222,#5420);
#4477=LINE('',#38224,#5421);
#4478=LINE('',#38225,#5422);
#4479=LINE('',#38227,#5423);
#4480=LINE('',#38228,#5424);
#4481=LINE('',#38230,#5425);
#4482=LINE('',#38231,#5426);
#4483=LINE('',#38233,#5427);
#4484=LINE('',#38234,#5428);
#4485=LINE('',#38236,#5429);
#4486=LINE('',#38237,#5430);
#4487=LINE('',#38239,#5431);
#4488=LINE('',#38240,#5432);
#4489=LINE('',#38242,#5433);
#4490=LINE('',#38243,#5434);
#4491=LINE('',#38245,#5435);
#4492=LINE('',#38246,#5436);
#4493=LINE('',#38248,#5437);
#4494=LINE('',#38249,#5438);
#4495=LINE('',#38251,#5439);
#4496=LINE('',#38252,#5440);
#4497=LINE('',#38254,#5441);
#4498=LINE('',#38255,#5442);
#4499=LINE('',#38257,#5443);
#4500=LINE('',#38258,#5444);
#4501=LINE('',#38260,#5445);
#4502=LINE('',#38261,#5446);
#4503=LINE('',#38263,#5447);
#4504=LINE('',#38264,#5448);
#4505=LINE('',#38266,#5449);
#4506=LINE('',#38267,#5450);
#4507=LINE('',#38269,#5451);
#4508=LINE('',#38270,#5452);
#4509=LINE('',#38272,#5453);
#4510=LINE('',#38273,#5454);
#4511=LINE('',#38275,#5455);
#4512=LINE('',#38276,#5456);
#4513=LINE('',#38278,#5457);
#4514=LINE('',#38279,#5458);
#4515=LINE('',#38281,#5459);
#4516=LINE('',#38282,#5460);
#4517=LINE('',#38284,#5461);
#4518=LINE('',#38285,#5462);
#4519=LINE('',#38287,#5463);
#4520=LINE('',#38288,#5464);
#4521=LINE('',#38290,#5465);
#4522=LINE('',#38291,#5466);
#4523=LINE('',#38293,#5467);
#4524=LINE('',#38294,#5468);
#4525=LINE('',#38296,#5469);
#4526=LINE('',#38297,#5470);
#4527=LINE('',#38299,#5471);
#4528=LINE('',#38300,#5472);
#4529=LINE('',#38302,#5473);
#4530=LINE('',#38303,#5474);
#4531=LINE('',#38305,#5475);
#4532=LINE('',#38306,#5476);
#4533=LINE('',#38308,#5477);
#4534=LINE('',#38309,#5478);
#4535=LINE('',#38311,#5479);
#4536=LINE('',#38312,#5480);
#4537=LINE('',#38314,#5481);
#4538=LINE('',#38315,#5482);
#4539=LINE('',#38317,#5483);
#4540=LINE('',#38318,#5484);
#4541=LINE('',#38320,#5485);
#4542=LINE('',#38321,#5486);
#4543=LINE('',#38323,#5487);
#4544=LINE('',#38324,#5488);
#4545=LINE('',#38326,#5489);
#4546=LINE('',#38327,#5490);
#4547=LINE('',#38329,#5491);
#4548=LINE('',#38330,#5492);
#4549=LINE('',#38332,#5493);
#4550=LINE('',#38333,#5494);
#4551=LINE('',#38335,#5495);
#4552=LINE('',#38336,#5496);
#4553=LINE('',#38338,#5497);
#4554=LINE('',#38339,#5498);
#4555=LINE('',#38341,#5499);
#4556=LINE('',#38342,#5500);
#4557=LINE('',#38344,#5501);
#4558=LINE('',#38345,#5502);
#4559=LINE('',#38347,#5503);
#4560=LINE('',#38348,#5504);
#4561=LINE('',#38350,#5505);
#4562=LINE('',#38351,#5506);
#4563=LINE('',#38354,#5507);
#4564=LINE('',#38355,#5508);
#4565=LINE('',#38360,#5509);
#4566=LINE('',#38363,#5510);
#4567=LINE('',#38366,#5511);
#4568=LINE('',#38369,#5512);
#4569=LINE('',#38372,#5513);
#4570=LINE('',#38375,#5514);
#4571=LINE('',#38378,#5515);
#4572=LINE('',#38381,#5516);
#4573=LINE('',#38384,#5517);
#4574=LINE('',#38387,#5518);
#4575=LINE('',#38390,#5519);
#4576=LINE('',#38393,#5520);
#4577=LINE('',#38396,#5521);
#4578=LINE('',#38399,#5522);
#4579=LINE('',#38402,#5523);
#4580=LINE('',#38405,#5524);
#4581=LINE('',#38408,#5525);
#4582=LINE('',#38411,#5526);
#4583=LINE('',#38414,#5527);
#4584=LINE('',#38417,#5528);
#4585=LINE('',#38420,#5529);
#4586=LINE('',#38423,#5530);
#4587=LINE('',#38426,#5531);
#4588=LINE('',#38429,#5532);
#4589=LINE('',#38432,#5533);
#4590=LINE('',#38435,#5534);
#4591=LINE('',#38438,#5535);
#4592=LINE('',#38441,#5536);
#4593=LINE('',#38444,#5537);
#4594=LINE('',#38447,#5538);
#4595=LINE('',#38450,#5539);
#4596=LINE('',#38453,#5540);
#4597=LINE('',#38456,#5541);
#4598=LINE('',#38459,#5542);
#4599=LINE('',#38462,#5543);
#4600=LINE('',#38465,#5544);
#4601=LINE('',#38468,#5545);
#4602=LINE('',#38471,#5546);
#4603=LINE('',#38474,#5547);
#4604=LINE('',#38477,#5548);
#4605=LINE('',#38480,#5549);
#4606=LINE('',#38483,#5550);
#4607=LINE('',#38486,#5551);
#4608=LINE('',#38489,#5552);
#4609=LINE('',#38492,#5553);
#4610=LINE('',#38495,#5554);
#4611=LINE('',#38498,#5555);
#4612=LINE('',#38501,#5556);
#4613=LINE('',#38504,#5557);
#4614=LINE('',#38507,#5558);
#4615=LINE('',#38510,#5559);
#4616=LINE('',#38513,#5560);
#4617=LINE('',#38516,#5561);
#4618=LINE('',#38519,#5562);
#4619=LINE('',#38522,#5563);
#4620=LINE('',#38525,#5564);
#4621=LINE('',#38528,#5565);
#4622=LINE('',#38531,#5566);
#4623=LINE('',#38534,#5567);
#4624=LINE('',#38537,#5568);
#4625=LINE('',#38540,#5569);
#4626=LINE('',#38543,#5570);
#4627=LINE('',#38546,#5571);
#4628=LINE('',#38549,#5572);
#4629=LINE('',#38552,#5573);
#4630=LINE('',#38555,#5574);
#4631=LINE('',#38558,#5575);
#4632=LINE('',#38561,#5576);
#4633=LINE('',#38564,#5577);
#4634=LINE('',#38567,#5578);
#4635=LINE('',#38570,#5579);
#4636=LINE('',#38573,#5580);
#4637=LINE('',#38576,#5581);
#4638=LINE('',#38579,#5582);
#4639=LINE('',#38582,#5583);
#4640=LINE('',#38585,#5584);
#4641=LINE('',#38588,#5585);
#4642=VECTOR('',#19751,1000.);
#4643=VECTOR('',#19754,1000.);
#4644=VECTOR('',#19759,1000.);
#4645=VECTOR('',#19762,1000.);
#4646=VECTOR('',#19765,1000.);
#4647=VECTOR('',#19766,1000.);
#4648=VECTOR('',#19767,1000.);
#4649=VECTOR('',#19768,1000.);
#4650=VECTOR('',#19769,1000.);
#4651=VECTOR('',#19770,1000.);
#4652=VECTOR('',#19773,1000.);
#4653=VECTOR('',#19774,1000.);
#4654=VECTOR('',#19775,1000.);
#4655=VECTOR('',#19776,1000.);
#4656=VECTOR('',#19777,1000.);
#4657=VECTOR('',#19778,1000.);
#4658=VECTOR('',#19803,1000.);
#4659=VECTOR('',#19806,1000.);
#4660=VECTOR('',#19811,1000.);
#4661=VECTOR('',#19814,1000.);
#4662=VECTOR('',#19819,1000.);
#4663=VECTOR('',#19822,1000.);
#4664=VECTOR('',#19825,1000.);
#4665=VECTOR('',#19826,1000.);
#4666=VECTOR('',#19827,1000.);
#4667=VECTOR('',#19828,1000.);
#4668=VECTOR('',#19829,1000.);
#4669=VECTOR('',#19832,1000.);
#4670=VECTOR('',#19833,1000.);
#4671=VECTOR('',#19834,1000.);
#4672=VECTOR('',#19835,1000.);
#4673=VECTOR('',#19836,1000.);
#4674=VECTOR('',#19853,1000.);
#4675=VECTOR('',#19854,1000.);
#4676=VECTOR('',#19855,1000.);
#4677=VECTOR('',#19856,1000.);
#4678=VECTOR('',#19859,1000.);
#4679=VECTOR('',#19860,1000.);
#4680=VECTOR('',#19861,1000.);
#4681=VECTOR('',#19862,1000.);
#4682=VECTOR('',#19863,1000.);
#4683=VECTOR('',#19864,1000.);
#4684=VECTOR('',#19865,1000.);
#4685=VECTOR('',#19868,1000.);
#4686=VECTOR('',#19869,1000.);
#4687=VECTOR('',#19870,1000.);
#4688=VECTOR('',#19871,1000.);
#4689=VECTOR('',#19872,1000.);
#4690=VECTOR('',#19873,1000.);
#4691=VECTOR('',#19874,1000.);
#4692=VECTOR('',#19903,1000.);
#4693=VECTOR('',#19904,1000.);
#4694=VECTOR('',#19905,1000.);
#4695=VECTOR('',#19906,1000.);
#4696=VECTOR('',#19909,1000.);
#4697=VECTOR('',#19910,1000.);
#4698=VECTOR('',#19911,1000.);
#4699=VECTOR('',#19912,1000.);
#4700=VECTOR('',#19913,1000.);
#4701=VECTOR('',#19914,1000.);
#4702=VECTOR('',#19915,1000.);
#4703=VECTOR('',#19918,1000.);
#4704=VECTOR('',#19919,1000.);
#4705=VECTOR('',#19920,1000.);
#4706=VECTOR('',#19921,1000.);
#4707=VECTOR('',#19922,1000.);
#4708=VECTOR('',#19923,1000.);
#4709=VECTOR('',#19924,1000.);
#4710=VECTOR('',#19957,1000.);
#4711=VECTOR('',#19960,1000.);
#4712=VECTOR('',#19965,1000.);
#4713=VECTOR('',#19968,1000.);
#4714=VECTOR('',#19969,1000.);
#4715=VECTOR('',#19970,1000.);
#4716=VECTOR('',#19971,1000.);
#4717=VECTOR('',#19972,1000.);
#4718=VECTOR('',#19985,1000.);
#4719=VECTOR('',#19988,1000.);
#4720=VECTOR('',#19993,1000.);
#4721=VECTOR('',#19996,1000.);
#4722=VECTOR('',#19999,1000.);
#4723=VECTOR('',#20002,1000.);
#4724=VECTOR('',#20003,1000.);
#4725=VECTOR('',#20004,1000.);
#4726=VECTOR('',#20011,1000.);
#4727=VECTOR('',#20012,1000.);
#4728=VECTOR('',#20013,1000.);
#4729=VECTOR('',#20014,1000.);
#4730=VECTOR('',#20017,1000.);
#4731=VECTOR('',#20018,1000.);
#4732=VECTOR('',#20019,1000.);
#4733=VECTOR('',#20020,1000.);
#4734=VECTOR('',#20021,1000.);
#4735=VECTOR('',#20022,1000.);
#4736=VECTOR('',#20023,1000.);
#4737=VECTOR('',#20026,1000.);
#4738=VECTOR('',#20027,1000.);
#4739=VECTOR('',#20028,1000.);
#4740=VECTOR('',#20031,1000.);
#4741=VECTOR('',#20032,1000.);
#4742=VECTOR('',#20033,1000.);
#4743=VECTOR('',#20034,1000.);
#4744=VECTOR('',#20035,1000.);
#4745=VECTOR('',#20036,1000.);
#4746=VECTOR('',#20059,2.6);
#4747=VECTOR('',#20064,2.6);
#4748=VECTOR('',#20069,7.);
#4749=VECTOR('',#20078,8.69677462715879);
#4750=VECTOR('',#20085,8.);
#4751=VECTOR('',#20090,10.);
#4752=VECTOR('',#20101,4.29685191531258);
#4753=VECTOR('',#20102,1000.);
#4754=VECTOR('',#20105,4.29685191531258);
#4755=VECTOR('',#20108,4.29685191531258);
#4756=VECTOR('',#20111,4.29685191531258);
#4757=VECTOR('',#20114,4.29685191531258);
#4758=VECTOR('',#20117,4.29685191531258);
#4759=VECTOR('',#20120,4.29685191531258);
#4760=VECTOR('',#20123,4.29685191531258);
#4761=VECTOR('',#20126,4.29685191531258);
#4762=VECTOR('',#20129,4.29685191531258);
#4763=VECTOR('',#20132,4.29685191531258);
#4764=VECTOR('',#20135,4.29685191531258);
#4765=VECTOR('',#20138,4.29685191531258);
#4766=VECTOR('',#20141,4.29685191531258);
#4767=VECTOR('',#20144,4.29685191531258);
#4768=VECTOR('',#20147,4.29685191531258);
#4769=VECTOR('',#20150,4.29685191531258);
#4770=VECTOR('',#20153,4.29685191531258);
#4771=VECTOR('',#20156,4.29685191531258);
#4772=VECTOR('',#20159,4.29685191531258);
#4773=VECTOR('',#20162,4.29685191531258);
#4774=VECTOR('',#20165,4.29685191531258);
#4775=VECTOR('',#20168,4.29685191531258);
#4776=VECTOR('',#20171,4.29685191531258);
#4777=VECTOR('',#20174,4.29685191531258);
#4778=VECTOR('',#20179,4.12499999999999);
#4779=VECTOR('',#20184,4.12499999999999);
#4780=VECTOR('',#20185,1000.);
#4781=VECTOR('',#20190,4.12499999999999);
#4782=VECTOR('',#20193,4.12499999999999);
#4783=VECTOR('',#20196,4.12499999999999);
#4784=VECTOR('',#20199,4.12499999999999);
#4785=VECTOR('',#20202,4.12499999999999);
#4786=VECTOR('',#20205,4.12499999999999);
#4787=VECTOR('',#20208,4.12499999999999);
#4788=VECTOR('',#20211,4.12499999999999);
#4789=VECTOR('',#20214,4.12499999999999);
#4790=VECTOR('',#20217,4.12499999999999);
#4791=VECTOR('',#20220,4.12499999999999);
#4792=VECTOR('',#20223,4.12499999999999);
#4793=VECTOR('',#20226,4.12499999999999);
#4794=VECTOR('',#20229,4.12499999999999);
#4795=VECTOR('',#20232,4.12499999999999);
#4796=VECTOR('',#20235,4.12499999999999);
#4797=VECTOR('',#20238,4.12499999999999);
#4798=VECTOR('',#20241,4.12499999999999);
#4799=VECTOR('',#20244,4.12499999999999);
#4800=VECTOR('',#20247,4.12499999999999);
#4801=VECTOR('',#20250,4.12499999999999);
#4802=VECTOR('',#20253,4.12499999999999);
#4803=VECTOR('',#20256,4.12499999999999);
#4804=VECTOR('',#20261,4.15);
#4805=VECTOR('',#20268,8.);
#4806=VECTOR('',#20273,8.);
#4807=VECTOR('',#20292,12.5);
#4808=VECTOR('',#20297,12.5);
#4809=VECTOR('',#20314,25.);
#4810=VECTOR('',#20319,22.5);
#4811=VECTOR('',#20334,10.);
#4812=VECTOR('',#20335,10.);
#4813=VECTOR('',#20338,10.);
#4814=VECTOR('',#20339,10.);
#4815=VECTOR('',#20344,1000.);
#4816=VECTOR('',#20345,1000.);
#4817=VECTOR('',#20354,8.05);
#4818=VECTOR('',#20361,10.5);
#4819=VECTOR('',#20376,22.5);
#4820=VECTOR('',#20383,25.);
#4821=VECTOR('',#20412,2.5);
#4822=VECTOR('',#20417,3.);
#4823=VECTOR('',#20434,10.);
#4824=VECTOR('',#20439,10.);
#4825=VECTOR('',#20446,4.);
#4826=VECTOR('',#20451,4.);
#4827=VECTOR('',#20462,5.);
#4828=VECTOR('',#20477,7.85653654166145);
#4829=VECTOR('',#20498,1000.);
#4830=VECTOR('',#20501,1000.);
#4831=VECTOR('',#20520,12.25);
#4832=VECTOR('',#20533,1000.);
#4833=VECTOR('',#20534,6.);
#4834=VECTOR('',#20537,1000.);
#4835=VECTOR('',#20550,1000.);
#4836=VECTOR('',#20551,1000.);
#4837=VECTOR('',#20556,1000.);
#4838=VECTOR('',#20563,1000.);
#4839=VECTOR('',#20570,1000.);
#4840=VECTOR('',#20573,1000.);
#4841=VECTOR('',#20638,6.);
#4842=VECTOR('',#20651,6.);
#4843=VECTOR('',#20656,6.);
#4844=VECTOR('',#20661,5.5);
#4845=VECTOR('',#20684,1000.);
#4846=VECTOR('',#20689,1000.);
#4847=VECTOR('',#20694,4.94835215326525);
#4848=VECTOR('',#20717,4.);
#4849=VECTOR('',#20724,6.72023753462643);
#4850=VECTOR('',#20745,1000.);
#4851=VECTOR('',#20752,1000.);
#4852=VECTOR('',#20787,6.);
#4853=VECTOR('',#20800,4.);
#4854=VECTOR('',#20805,4.);
#4855=VECTOR('',#20810,3.5);
#4856=VECTOR('',#20835,4.25);
#4857=VECTOR('',#20844,5.);
#4858=VECTOR('',#20847,5.);
#4859=VECTOR('',#20856,4.25);
#4860=VECTOR('',#20861,6.);
#4861=VECTOR('',#20866,12.5);
#4862=VECTOR('',#20893,1000.);
#4863=VECTOR('',#20896,1000.);
#4864=VECTOR('',#20921,1000.);
#4865=VECTOR('',#20924,1000.);
#4866=VECTOR('',#20939,1000.);
#4867=VECTOR('',#20942,1000.);
#4868=VECTOR('',#20967,1000.);
#4869=VECTOR('',#20970,1000.);
#4870=VECTOR('',#20973,1000.);
#4871=VECTOR('',#20978,1000.);
#4872=VECTOR('',#20983,1000.);
#4873=VECTOR('',#20986,1000.);
#4874=VECTOR('',#20991,5.);
#4875=VECTOR('',#20998,12.5);
#4876=VECTOR('',#21005,1000.);
#4877=VECTOR('',#21008,1000.);
#4878=VECTOR('',#21013,1000.);
#4879=VECTOR('',#21026,1000.);
#4880=VECTOR('',#21033,1000.);
#4881=VECTOR('',#21036,1000.);
#4882=VECTOR('',#21133,1000.);
#4883=VECTOR('',#21134,1000.);
#4884=VECTOR('',#21163,1000.);
#4885=VECTOR('',#21166,1000.);
#4886=VECTOR('',#21169,1000.);
#4887=VECTOR('',#21174,1000.);
#4888=VECTOR('',#21315,2.);
#4889=VECTOR('',#21324,1.80000000000002);
#4890=VECTOR('',#21333,2.3);
#4891=VECTOR('',#21340,1.2);
#4892=VECTOR('',#21355,1.50000000000001);
#4893=VECTOR('',#21364,2.3);
#4894=VECTOR('',#21371,2.);
#4895=VECTOR('',#21378,1.5);
#4896=VECTOR('',#21389,2.);
#4897=VECTOR('',#21398,2.);
#4898=VECTOR('',#21401,1.2);
#4899=VECTOR('',#21404,1000.);
#4900=VECTOR('',#21405,1000.);
#4901=VECTOR('',#21406,1000.);
#4902=VECTOR('',#21409,2.);
#4903=VECTOR('',#21412,1.5);
#4904=VECTOR('',#21415,1000.);
#4905=VECTOR('',#21416,1000.);
#4906=VECTOR('',#21417,1000.);
#4907=VECTOR('',#21418,1000.);
#4908=VECTOR('',#21421,1000.);
#4909=VECTOR('',#21422,1000.);
#4910=VECTOR('',#21423,1000.);
#4911=VECTOR('',#21424,1000.);
#4912=VECTOR('',#21427,1000.);
#4913=VECTOR('',#21430,1000.);
#4914=VECTOR('',#21431,1000.);
#4915=VECTOR('',#21432,1000.);
#4916=VECTOR('',#21433,1000.);
#4917=VECTOR('',#21434,1000.);
#4918=VECTOR('',#21435,1000.);
#4919=VECTOR('',#21436,1000.);
#4920=VECTOR('',#21437,1000.);
#4921=VECTOR('',#21438,1000.);
#4922=VECTOR('',#21439,1000.);
#4923=VECTOR('',#21442,1000.);
#4924=VECTOR('',#21445,1000.);
#4925=VECTOR('',#21446,1000.);
#4926=VECTOR('',#21447,1000.);
#4927=VECTOR('',#21450,1000.);
#4928=VECTOR('',#21451,1000.);
#4929=VECTOR('',#21454,1000.);
#4930=VECTOR('',#21455,1000.);
#4931=VECTOR('',#21456,1000.);
#4932=VECTOR('',#21457,1000.);
#4933=VECTOR('',#21458,1000.);
#4934=VECTOR('',#21459,1000.);
#4935=VECTOR('',#21460,1000.);
#4936=VECTOR('',#21461,1000.);
#4937=VECTOR('',#21462,1000.);
#4938=VECTOR('',#21463,1000.);
#4939=VECTOR('',#21464,1000.);
#4940=VECTOR('',#21465,1000.);
#4941=VECTOR('',#21466,1000.);
#4942=VECTOR('',#21471,1000.);
#4943=VECTOR('',#21472,1000.);
#4944=VECTOR('',#21473,1000.);
#4945=VECTOR('',#21474,1000.);
#4946=VECTOR('',#21477,1000.);
#4947=VECTOR('',#21478,1000.);
#4948=VECTOR('',#21479,1000.);
#4949=VECTOR('',#21480,1000.);
#4950=VECTOR('',#21481,1000.);
#4951=VECTOR('',#21482,1000.);
#4952=VECTOR('',#21483,1000.);
#4953=VECTOR('',#21486,1000.);
#4954=VECTOR('',#21487,1000.);
#4955=VECTOR('',#21488,1000.);
#4956=VECTOR('',#21489,1000.);
#4957=VECTOR('',#21492,1000.);
#4958=VECTOR('',#21493,1000.);
#4959=VECTOR('',#21496,1000.);
#4960=VECTOR('',#21497,1000.);
#4961=VECTOR('',#21498,1000.);
#4962=VECTOR('',#21499,1000.);
#4963=VECTOR('',#21502,1000.);
#4964=VECTOR('',#21503,1000.);
#4965=VECTOR('',#21504,1000.);
#4966=VECTOR('',#21505,1000.);
#4967=VECTOR('',#21508,1000.);
#4968=VECTOR('',#21511,1000.);
#4969=VECTOR('',#21518,1000.);
#4970=VECTOR('',#21521,1000.);
#4971=VECTOR('',#21528,1000.);
#4972=VECTOR('',#21531,1000.);
#4973=VECTOR('',#21536,1000.);
#4974=VECTOR('',#21539,1000.);
#4975=VECTOR('',#21544,1000.);
#4976=VECTOR('',#21545,1000.);
#4977=VECTOR('',#21548,1000.);
#4978=VECTOR('',#21549,1000.);
#4979=VECTOR('',#21552,1000.);
#4980=VECTOR('',#21553,1000.);
#4981=VECTOR('',#21556,1000.);
#4982=VECTOR('',#21557,1000.);
#4983=VECTOR('',#21558,1000.);
#4984=VECTOR('',#21561,1000.);
#4985=VECTOR('',#21562,1000.);
#4986=VECTOR('',#21569,1000.);
#4987=VECTOR('',#21570,1000.);
#4988=VECTOR('',#21575,1000.);
#4989=VECTOR('',#21576,1000.);
#4990=VECTOR('',#21577,1000.);
#4991=VECTOR('',#21734,1.2);
#4992=VECTOR('',#21743,2.5);
#4993=VECTOR('',#21752,3.);
#4994=VECTOR('',#21761,4.25);
#4995=VECTOR('',#21768,1.2);
#4996=VECTOR('',#21775,1.2);
#4997=VECTOR('',#21782,2.);
#4998=VECTOR('',#21787,1000.);
#4999=VECTOR('',#21788,1000.);
#5000=VECTOR('',#21789,1000.);
#5001=VECTOR('',#21792,1000.);
#5002=VECTOR('',#21795,1000.);
#5003=VECTOR('',#21800,1000.);
#5004=VECTOR('',#21801,1000.);
#5005=VECTOR('',#21802,1000.);
#5006=VECTOR('',#21805,1000.);
#5007=VECTOR('',#21806,1000.);
#5008=VECTOR('',#21809,1000.);
#5009=VECTOR('',#21810,1000.);
#5010=VECTOR('',#21811,1000.);
#5011=VECTOR('',#21814,1000.);
#5012=VECTOR('',#21817,1000.);
#5013=VECTOR('',#21818,1000.);
#5014=VECTOR('',#21821,1000.);
#5015=VECTOR('',#21822,1000.);
#5016=VECTOR('',#21823,1000.);
#5017=VECTOR('',#21824,1000.);
#5018=VECTOR('',#21827,1000.);
#5019=VECTOR('',#21832,1000.);
#5020=VECTOR('',#21833,1000.);
#5021=VECTOR('',#21836,1000.);
#5022=VECTOR('',#21837,1000.);
#5023=VECTOR('',#21838,1000.);
#5024=VECTOR('',#21841,1000.);
#5025=VECTOR('',#21844,1000.);
#5026=VECTOR('',#21857,2.5);
#5027=VECTOR('',#21880,2.);
#5028=VECTOR('',#21889,1.61);
#5029=VECTOR('',#21896,2.);
#5030=VECTOR('',#21903,2.);
#5031=VECTOR('',#21910,1.61);
#5032=VECTOR('',#21917,2.);
#5033=VECTOR('',#21924,2.);
#5034=VECTOR('',#21931,1.61);
#5035=VECTOR('',#21938,2.);
#5036=VECTOR('',#21945,2.);
#5037=VECTOR('',#21952,1.61);
#5038=VECTOR('',#21959,2.);
#5039=VECTOR('',#21966,2.);
#5040=VECTOR('',#21973,1.61);
#5041=VECTOR('',#21980,2.);
#5042=VECTOR('',#21987,2.);
#5043=VECTOR('',#21994,1.61);
#5044=VECTOR('',#22001,2.);
#5045=VECTOR('',#22008,2.);
#5046=VECTOR('',#22015,1.61);
#5047=VECTOR('',#22022,2.);
#5048=VECTOR('',#22029,2.);
#5049=VECTOR('',#22036,1.61);
#5050=VECTOR('',#22043,2.);
#5051=VECTOR('',#22050,2.);
#5052=VECTOR('',#22057,1.61);
#5053=VECTOR('',#22064,2.);
#5054=VECTOR('',#22071,2.);
#5055=VECTOR('',#22078,1.61);
#5056=VECTOR('',#22085,2.);
#5057=VECTOR('',#22092,2.);
#5058=VECTOR('',#22099,1.61);
#5059=VECTOR('',#22106,2.);
#5060=VECTOR('',#22113,2.);
#5061=VECTOR('',#22120,1.61);
#5062=VECTOR('',#22127,2.);
#5063=VECTOR('',#22134,2.);
#5064=VECTOR('',#22141,1.61);
#5065=VECTOR('',#22148,2.);
#5066=VECTOR('',#22155,2.);
#5067=VECTOR('',#22162,1.61);
#5068=VECTOR('',#22169,2.);
#5069=VECTOR('',#22176,2.);
#5070=VECTOR('',#22183,1.61);
#5071=VECTOR('',#22190,2.);
#5072=VECTOR('',#22271,8.175);
#5073=VECTOR('',#22430,8.175);
#5074=VECTOR('',#22511,2.);
#5075=VECTOR('',#22514,1000.);
#5076=VECTOR('',#22515,1000.);
#5077=VECTOR('',#22518,1000.);
#5078=VECTOR('',#22519,1000.);
#5079=VECTOR('',#22522,1000.);
#5080=VECTOR('',#22523,1000.);
#5081=VECTOR('',#22526,1000.);
#5082=VECTOR('',#22527,1000.);
#5083=VECTOR('',#22530,1000.);
#5084=VECTOR('',#22531,1000.);
#5085=VECTOR('',#22534,1000.);
#5086=VECTOR('',#22535,1000.);
#5087=VECTOR('',#22538,1000.);
#5088=VECTOR('',#22539,1000.);
#5089=VECTOR('',#22542,1000.);
#5090=VECTOR('',#22543,1000.);
#5091=VECTOR('',#22546,1000.);
#5092=VECTOR('',#22547,1000.);
#5093=VECTOR('',#22550,1000.);
#5094=VECTOR('',#22551,1000.);
#5095=VECTOR('',#22554,1000.);
#5096=VECTOR('',#22555,1000.);
#5097=VECTOR('',#22558,1000.);
#5098=VECTOR('',#22559,1000.);
#5099=VECTOR('',#22562,1000.);
#5100=VECTOR('',#22563,1000.);
#5101=VECTOR('',#22566,1000.);
#5102=VECTOR('',#22567,1000.);
#5103=VECTOR('',#22570,1000.);
#5104=VECTOR('',#22571,1000.);
#5105=VECTOR('',#22574,1000.);
#5106=VECTOR('',#22575,1000.);
#5107=VECTOR('',#22578,1000.);
#5108=VECTOR('',#22579,1000.);
#5109=VECTOR('',#22582,1000.);
#5110=VECTOR('',#22583,1000.);
#5111=VECTOR('',#22586,1000.);
#5112=VECTOR('',#22587,1000.);
#5113=VECTOR('',#22590,1000.);
#5114=VECTOR('',#22591,1000.);
#5115=VECTOR('',#22594,1000.);
#5116=VECTOR('',#22595,1000.);
#5117=VECTOR('',#22598,1000.);
#5118=VECTOR('',#22599,1000.);
#5119=VECTOR('',#22602,1000.);
#5120=VECTOR('',#22603,1000.);
#5121=VECTOR('',#22606,1000.);
#5122=VECTOR('',#22607,1000.);
#5123=VECTOR('',#22610,1000.);
#5124=VECTOR('',#22611,1000.);
#5125=VECTOR('',#22614,1000.);
#5126=VECTOR('',#22615,1000.);
#5127=VECTOR('',#22618,1000.);
#5128=VECTOR('',#22619,1000.);
#5129=VECTOR('',#22622,1000.);
#5130=VECTOR('',#22623,1000.);
#5131=VECTOR('',#22626,1000.);
#5132=VECTOR('',#22627,1000.);
#5133=VECTOR('',#22630,1000.);
#5134=VECTOR('',#22631,1000.);
#5135=VECTOR('',#22634,1000.);
#5136=VECTOR('',#22635,1000.);
#5137=VECTOR('',#22638,1000.);
#5138=VECTOR('',#22639,1000.);
#5139=VECTOR('',#22642,1000.);
#5140=VECTOR('',#22643,1000.);
#5141=VECTOR('',#22646,1000.);
#5142=VECTOR('',#22647,1000.);
#5143=VECTOR('',#22650,1000.);
#5144=VECTOR('',#22651,1000.);
#5145=VECTOR('',#22654,1000.);
#5146=VECTOR('',#22655,1000.);
#5147=VECTOR('',#22658,1000.);
#5148=VECTOR('',#22659,1000.);
#5149=VECTOR('',#22662,1000.);
#5150=VECTOR('',#22663,1000.);
#5151=VECTOR('',#22666,1000.);
#5152=VECTOR('',#22667,1000.);
#5153=VECTOR('',#22670,1000.);
#5154=VECTOR('',#22671,1000.);
#5155=VECTOR('',#22674,1000.);
#5156=VECTOR('',#22675,1000.);
#5157=VECTOR('',#22678,1000.);
#5158=VECTOR('',#22679,1000.);
#5159=VECTOR('',#22682,1000.);
#5160=VECTOR('',#22683,1000.);
#5161=VECTOR('',#22686,1000.);
#5162=VECTOR('',#22687,1000.);
#5163=VECTOR('',#22690,1000.);
#5164=VECTOR('',#22691,1000.);
#5165=VECTOR('',#22694,1000.);
#5166=VECTOR('',#22695,1000.);
#5167=VECTOR('',#22698,1000.);
#5168=VECTOR('',#22699,1000.);
#5169=VECTOR('',#22702,1000.);
#5170=VECTOR('',#22703,1000.);
#5171=VECTOR('',#22706,1000.);
#5172=VECTOR('',#22707,1000.);
#5173=VECTOR('',#22710,1000.);
#5174=VECTOR('',#22711,1000.);
#5175=VECTOR('',#22714,1000.);
#5176=VECTOR('',#22715,1000.);
#5177=VECTOR('',#22718,1000.);
#5178=VECTOR('',#22719,1000.);
#5179=VECTOR('',#22722,1000.);
#5180=VECTOR('',#22723,1000.);
#5181=VECTOR('',#22726,1000.);
#5182=VECTOR('',#22727,1000.);
#5183=VECTOR('',#22730,1000.);
#5184=VECTOR('',#22731,1000.);
#5185=VECTOR('',#22734,1000.);
#5186=VECTOR('',#22735,1000.);
#5187=VECTOR('',#22738,1000.);
#5188=VECTOR('',#22739,1000.);
#5189=VECTOR('',#22742,1000.);
#5190=VECTOR('',#22743,1000.);
#5191=VECTOR('',#22746,1000.);
#5192=VECTOR('',#22747,1000.);
#5193=VECTOR('',#22750,1000.);
#5194=VECTOR('',#22751,1000.);
#5195=VECTOR('',#22754,1000.);
#5196=VECTOR('',#22755,1000.);
#5197=VECTOR('',#22758,1000.);
#5198=VECTOR('',#22759,1000.);
#5199=VECTOR('',#22762,1000.);
#5200=VECTOR('',#22763,1000.);
#5201=VECTOR('',#22766,1000.);
#5202=VECTOR('',#22767,1000.);
#5203=VECTOR('',#22770,1000.);
#5204=VECTOR('',#22771,1000.);
#5205=VECTOR('',#22774,1000.);
#5206=VECTOR('',#22775,1000.);
#5207=VECTOR('',#22778,1000.);
#5208=VECTOR('',#22779,1000.);
#5209=VECTOR('',#22782,1000.);
#5210=VECTOR('',#22783,1000.);
#5211=VECTOR('',#22786,1000.);
#5212=VECTOR('',#22787,1000.);
#5213=VECTOR('',#22790,1000.);
#5214=VECTOR('',#22791,1000.);
#5215=VECTOR('',#22794,1000.);
#5216=VECTOR('',#22795,1000.);
#5217=VECTOR('',#22798,1000.);
#5218=VECTOR('',#22799,1000.);
#5219=VECTOR('',#22802,1000.);
#5220=VECTOR('',#22803,1000.);
#5221=VECTOR('',#22806,1000.);
#5222=VECTOR('',#22807,1000.);
#5223=VECTOR('',#22810,1000.);
#5224=VECTOR('',#22811,1000.);
#5225=VECTOR('',#22814,1000.);
#5226=VECTOR('',#22815,1000.);
#5227=VECTOR('',#22820,1000.);
#5228=VECTOR('',#22821,1000.);
#5229=VECTOR('',#22828,1000.);
#5230=VECTOR('',#22833,1000.);
#5231=VECTOR('',#22838,1000.);
#5232=VECTOR('',#22843,1000.);
#5233=VECTOR('',#22848,1000.);
#5234=VECTOR('',#22853,1000.);
#5235=VECTOR('',#22858,1000.);
#5236=VECTOR('',#22863,1000.);
#5237=VECTOR('',#22868,1000.);
#5238=VECTOR('',#22873,1000.);
#5239=VECTOR('',#22878,1000.);
#5240=VECTOR('',#22883,1000.);
#5241=VECTOR('',#22888,1000.);
#5242=VECTOR('',#22893,1000.);
#5243=VECTOR('',#22898,1000.);
#5244=VECTOR('',#22903,1000.);
#5245=VECTOR('',#22908,1000.);
#5246=VECTOR('',#22913,1000.);
#5247=VECTOR('',#22918,1000.);
#5248=VECTOR('',#22923,1000.);
#5249=VECTOR('',#22928,1000.);
#5250=VECTOR('',#22933,1000.);
#5251=VECTOR('',#22938,1000.);
#5252=VECTOR('',#22943,1000.);
#5253=VECTOR('',#22948,1000.);
#5254=VECTOR('',#22953,1000.);
#5255=VECTOR('',#22958,1000.);
#5256=VECTOR('',#22963,1000.);
#5257=VECTOR('',#22968,1000.);
#5258=VECTOR('',#22973,1000.);
#5259=VECTOR('',#22978,1000.);
#5260=VECTOR('',#22983,1000.);
#5261=VECTOR('',#22988,1000.);
#5262=VECTOR('',#22993,1000.);
#5263=VECTOR('',#22998,1000.);
#5264=VECTOR('',#23003,1000.);
#5265=VECTOR('',#23008,1000.);
#5266=VECTOR('',#23013,1000.);
#5267=VECTOR('',#23018,1000.);
#5268=VECTOR('',#23023,1000.);
#5269=VECTOR('',#23028,1000.);
#5270=VECTOR('',#23033,1000.);
#5271=VECTOR('',#23038,1000.);
#5272=VECTOR('',#23043,1000.);
#5273=VECTOR('',#23048,1000.);
#5274=VECTOR('',#23053,1000.);
#5275=VECTOR('',#23058,1000.);
#5276=VECTOR('',#23063,1000.);
#5277=VECTOR('',#23068,1000.);
#5278=VECTOR('',#23073,1000.);
#5279=VECTOR('',#23078,1000.);
#5280=VECTOR('',#23083,1000.);
#5281=VECTOR('',#23088,1000.);
#5282=VECTOR('',#23093,1000.);
#5283=VECTOR('',#23098,1000.);
#5284=VECTOR('',#23103,1000.);
#5285=VECTOR('',#23108,1000.);
#5286=VECTOR('',#23113,1000.);
#5287=VECTOR('',#23118,1000.);
#5288=VECTOR('',#23123,1000.);
#5289=VECTOR('',#23128,1000.);
#5290=VECTOR('',#23133,1000.);
#5291=VECTOR('',#23138,1000.);
#5292=VECTOR('',#23143,1000.);
#5293=VECTOR('',#23148,1000.);
#5294=VECTOR('',#23153,1000.);
#5295=VECTOR('',#23158,1000.);
#5296=VECTOR('',#23163,1000.);
#5297=VECTOR('',#23168,1000.);
#5298=VECTOR('',#23173,1000.);
#5299=VECTOR('',#23178,1000.);
#5300=VECTOR('',#23183,1000.);
#5301=VECTOR('',#23188,1000.);
#5302=VECTOR('',#23193,1000.);
#5303=VECTOR('',#23198,1000.);
#5304=VECTOR('',#23203,1000.);
#5305=VECTOR('',#23208,1000.);
#5306=VECTOR('',#23233,2.64252040565333);
#5307=VECTOR('',#23238,1.5);
#5308=VECTOR('',#23243,1000.);
#5309=VECTOR('',#23248,1000.);
#5310=VECTOR('',#23253,1000.);
#5311=VECTOR('',#23256,1000.);
#5312=VECTOR('',#23273,2.);
#5313=VECTOR('',#23282,1.61);
#5314=VECTOR('',#23289,2.);
#5315=VECTOR('',#23296,2.);
#5316=VECTOR('',#23303,1.61);
#5317=VECTOR('',#23310,2.);
#5318=VECTOR('',#23317,2.);
#5319=VECTOR('',#23324,1.61);
#5320=VECTOR('',#23331,2.);
#5321=VECTOR('',#23338,2.);
#5322=VECTOR('',#23345,1.61);
#5323=VECTOR('',#23352,2.);
#5324=VECTOR('',#23359,2.);
#5325=VECTOR('',#23366,1.61);
#5326=VECTOR('',#23373,2.);
#5327=VECTOR('',#23380,2.);
#5328=VECTOR('',#23387,1.61);
#5329=VECTOR('',#23394,2.);
#5330=VECTOR('',#23401,2.);
#5331=VECTOR('',#23408,1.61);
#5332=VECTOR('',#23415,2.);
#5333=VECTOR('',#23422,2.);
#5334=VECTOR('',#23429,1.61);
#5335=VECTOR('',#23436,2.);
#5336=VECTOR('',#23443,2.);
#5337=VECTOR('',#23450,1.61);
#5338=VECTOR('',#23457,2.);
#5339=VECTOR('',#23464,2.);
#5340=VECTOR('',#23471,1.61);
#5341=VECTOR('',#23478,2.);
#5342=VECTOR('',#23485,2.);
#5343=VECTOR('',#23492,1.61);
#5344=VECTOR('',#23499,2.);
#5345=VECTOR('',#23506,2.);
#5346=VECTOR('',#23513,1.61);
#5347=VECTOR('',#23520,2.);
#5348=VECTOR('',#23527,2.);
#5349=VECTOR('',#23534,1.61);
#5350=VECTOR('',#23541,2.);
#5351=VECTOR('',#23544,4.);
#5352=VECTOR('',#23627,8.175);
#5353=VECTOR('',#23786,8.175);
#5354=VECTOR('',#23869,2.);
#5355=VECTOR('',#23872,1000.);
#5356=VECTOR('',#23873,1000.);
#5357=VECTOR('',#23876,1000.);
#5358=VECTOR('',#23877,1000.);
#5359=VECTOR('',#23880,1000.);
#5360=VECTOR('',#23881,1000.);
#5361=VECTOR('',#23884,1000.);
#5362=VECTOR('',#23885,1000.);
#5363=VECTOR('',#23888,1000.);
#5364=VECTOR('',#23889,1000.);
#5365=VECTOR('',#23892,1000.);
#5366=VECTOR('',#23893,1000.);
#5367=VECTOR('',#23896,1000.);
#5368=VECTOR('',#23897,1000.);
#5369=VECTOR('',#23900,1000.);
#5370=VECTOR('',#23901,1000.);
#5371=VECTOR('',#23904,1000.);
#5372=VECTOR('',#23905,1000.);
#5373=VECTOR('',#23908,1000.);
#5374=VECTOR('',#23909,1000.);
#5375=VECTOR('',#23912,1000.);
#5376=VECTOR('',#23913,1000.);
#5377=VECTOR('',#23916,1000.);
#5378=VECTOR('',#23917,1000.);
#5379=VECTOR('',#23920,1000.);
#5380=VECTOR('',#23921,1000.);
#5381=VECTOR('',#23924,1000.);
#5382=VECTOR('',#23925,1000.);
#5383=VECTOR('',#23928,1000.);
#5384=VECTOR('',#23929,1000.);
#5385=VECTOR('',#23932,1000.);
#5386=VECTOR('',#23933,1000.);
#5387=VECTOR('',#23936,1000.);
#5388=VECTOR('',#23937,1000.);
#5389=VECTOR('',#23940,1000.);
#5390=VECTOR('',#23941,1000.);
#5391=VECTOR('',#23944,1000.);
#5392=VECTOR('',#23945,1000.);
#5393=VECTOR('',#23948,1000.);
#5394=VECTOR('',#23949,1000.);
#5395=VECTOR('',#23952,1000.);
#5396=VECTOR('',#23953,1000.);
#5397=VECTOR('',#23956,1000.);
#5398=VECTOR('',#23957,1000.);
#5399=VECTOR('',#23960,1000.);
#5400=VECTOR('',#23961,1000.);
#5401=VECTOR('',#23964,1000.);
#5402=VECTOR('',#23965,1000.);
#5403=VECTOR('',#23968,1000.);
#5404=VECTOR('',#23969,1000.);
#5405=VECTOR('',#23972,1000.);
#5406=VECTOR('',#23973,1000.);
#5407=VECTOR('',#23976,1000.);
#5408=VECTOR('',#23977,1000.);
#5409=VECTOR('',#23980,1000.);
#5410=VECTOR('',#23981,1000.);
#5411=VECTOR('',#23984,1000.);
#5412=VECTOR('',#23985,1000.);
#5413=VECTOR('',#23988,1000.);
#5414=VECTOR('',#23989,1000.);
#5415=VECTOR('',#23992,1000.);
#5416=VECTOR('',#23993,1000.);
#5417=VECTOR('',#23996,1000.);
#5418=VECTOR('',#23997,1000.);
#5419=VECTOR('',#24000,1000.);
#5420=VECTOR('',#24001,1000.);
#5421=VECTOR('',#24004,1000.);
#5422=VECTOR('',#24005,1000.);
#5423=VECTOR('',#24008,1000.);
#5424=VECTOR('',#24009,1000.);
#5425=VECTOR('',#24012,1000.);
#5426=VECTOR('',#24013,1000.);
#5427=VECTOR('',#24016,1000.);
#5428=VECTOR('',#24017,1000.);
#5429=VECTOR('',#24020,1000.);
#5430=VECTOR('',#24021,1000.);
#5431=VECTOR('',#24024,1000.);
#5432=VECTOR('',#24025,1000.);
#5433=VECTOR('',#24028,1000.);
#5434=VECTOR('',#24029,1000.);
#5435=VECTOR('',#24032,1000.);
#5436=VECTOR('',#24033,1000.);
#5437=VECTOR('',#24036,1000.);
#5438=VECTOR('',#24037,1000.);
#5439=VECTOR('',#24040,1000.);
#5440=VECTOR('',#24041,1000.);
#5441=VECTOR('',#24044,1000.);
#5442=VECTOR('',#24045,1000.);
#5443=VECTOR('',#24048,1000.);
#5444=VECTOR('',#24049,1000.);
#5445=VECTOR('',#24052,1000.);
#5446=VECTOR('',#24053,1000.);
#5447=VECTOR('',#24056,1000.);
#5448=VECTOR('',#24057,1000.);
#5449=VECTOR('',#24060,1000.);
#5450=VECTOR('',#24061,1000.);
#5451=VECTOR('',#24064,1000.);
#5452=VECTOR('',#24065,1000.);
#5453=VECTOR('',#24068,1000.);
#5454=VECTOR('',#24069,1000.);
#5455=VECTOR('',#24072,1000.);
#5456=VECTOR('',#24073,1000.);
#5457=VECTOR('',#24076,1000.);
#5458=VECTOR('',#24077,1000.);
#5459=VECTOR('',#24080,1000.);
#5460=VECTOR('',#24081,1000.);
#5461=VECTOR('',#24084,1000.);
#5462=VECTOR('',#24085,1000.);
#5463=VECTOR('',#24088,1000.);
#5464=VECTOR('',#24089,1000.);
#5465=VECTOR('',#24092,1000.);
#5466=VECTOR('',#24093,1000.);
#5467=VECTOR('',#24096,1000.);
#5468=VECTOR('',#24097,1000.);
#5469=VECTOR('',#24100,1000.);
#5470=VECTOR('',#24101,1000.);
#5471=VECTOR('',#24104,1000.);
#5472=VECTOR('',#24105,1000.);
#5473=VECTOR('',#24108,1000.);
#5474=VECTOR('',#24109,1000.);
#5475=VECTOR('',#24112,1000.);
#5476=VECTOR('',#24113,1000.);
#5477=VECTOR('',#24116,1000.);
#5478=VECTOR('',#24117,1000.);
#5479=VECTOR('',#24120,1000.);
#5480=VECTOR('',#24121,1000.);
#5481=VECTOR('',#24124,1000.);
#5482=VECTOR('',#24125,1000.);
#5483=VECTOR('',#24128,1000.);
#5484=VECTOR('',#24129,1000.);
#5485=VECTOR('',#24132,1000.);
#5486=VECTOR('',#24133,1000.);
#5487=VECTOR('',#24136,1000.);
#5488=VECTOR('',#24137,1000.);
#5489=VECTOR('',#24140,1000.);
#5490=VECTOR('',#24141,1000.);
#5491=VECTOR('',#24144,1000.);
#5492=VECTOR('',#24145,1000.);
#5493=VECTOR('',#24148,1000.);
#5494=VECTOR('',#24149,1000.);
#5495=VECTOR('',#24152,1000.);
#5496=VECTOR('',#24153,1000.);
#5497=VECTOR('',#24156,1000.);
#5498=VECTOR('',#24157,1000.);
#5499=VECTOR('',#24160,1000.);
#5500=VECTOR('',#24161,1000.);
#5501=VECTOR('',#24164,1000.);
#5502=VECTOR('',#24165,1000.);
#5503=VECTOR('',#24168,1000.);
#5504=VECTOR('',#24169,1000.);
#5505=VECTOR('',#24172,1000.);
#5506=VECTOR('',#24173,1000.);
#5507=VECTOR('',#24178,1000.);
#5508=VECTOR('',#24179,1000.);
#5509=VECTOR('',#24188,1000.);
#5510=VECTOR('',#24193,1000.);
#5511=VECTOR('',#24198,1000.);
#5512=VECTOR('',#24203,1000.);
#5513=VECTOR('',#24208,1000.);
#5514=VECTOR('',#24213,1000.);
#5515=VECTOR('',#24218,1000.);
#5516=VECTOR('',#24223,1000.);
#5517=VECTOR('',#24228,1000.);
#5518=VECTOR('',#24233,1000.);
#5519=VECTOR('',#24238,1000.);
#5520=VECTOR('',#24243,1000.);
#5521=VECTOR('',#24248,1000.);
#5522=VECTOR('',#24253,1000.);
#5523=VECTOR('',#24258,1000.);
#5524=VECTOR('',#24263,1000.);
#5525=VECTOR('',#24268,1000.);
#5526=VECTOR('',#24273,1000.);
#5527=VECTOR('',#24278,1000.);
#5528=VECTOR('',#24283,1000.);
#5529=VECTOR('',#24288,1000.);
#5530=VECTOR('',#24293,1000.);
#5531=VECTOR('',#24298,1000.);
#5532=VECTOR('',#24303,1000.);
#5533=VECTOR('',#24308,1000.);
#5534=VECTOR('',#24313,1000.);
#5535=VECTOR('',#24318,1000.);
#5536=VECTOR('',#24323,1000.);
#5537=VECTOR('',#24328,1000.);
#5538=VECTOR('',#24333,1000.);
#5539=VECTOR('',#24338,1000.);
#5540=VECTOR('',#24343,1000.);
#5541=VECTOR('',#24348,1000.);
#5542=VECTOR('',#24353,1000.);
#5543=VECTOR('',#24358,1000.);
#5544=VECTOR('',#24363,1000.);
#5545=VECTOR('',#24368,1000.);
#5546=VECTOR('',#24373,1000.);
#5547=VECTOR('',#24378,1000.);
#5548=VECTOR('',#24383,1000.);
#5549=VECTOR('',#24388,1000.);
#5550=VECTOR('',#24393,1000.);
#5551=VECTOR('',#24398,1000.);
#5552=VECTOR('',#24403,1000.);
#5553=VECTOR('',#24408,1000.);
#5554=VECTOR('',#24413,1000.);
#5555=VECTOR('',#24418,1000.);
#5556=VECTOR('',#24423,1000.);
#5557=VECTOR('',#24428,1000.);
#5558=VECTOR('',#24433,1000.);
#5559=VECTOR('',#24438,1000.);
#5560=VECTOR('',#24443,1000.);
#5561=VECTOR('',#24448,1000.);
#5562=VECTOR('',#24453,1000.);
#5563=VECTOR('',#24458,1000.);
#5564=VECTOR('',#24463,1000.);
#5565=VECTOR('',#24468,1000.);
#5566=VECTOR('',#24473,1000.);
#5567=VECTOR('',#24478,1000.);
#5568=VECTOR('',#24483,1000.);
#5569=VECTOR('',#24488,1000.);
#5570=VECTOR('',#24493,1000.);
#5571=VECTOR('',#24498,1000.);
#5572=VECTOR('',#24503,1000.);
#5573=VECTOR('',#24508,1000.);
#5574=VECTOR('',#24513,1000.);
#5575=VECTOR('',#24518,1000.);
#5576=VECTOR('',#24523,1000.);
#5577=VECTOR('',#24528,1000.);
#5578=VECTOR('',#24533,1000.);
#5579=VECTOR('',#24538,1000.);
#5580=VECTOR('',#24543,1000.);
#5581=VECTOR('',#24548,1000.);
#5582=VECTOR('',#24553,1000.);
#5583=VECTOR('',#24558,1000.);
#5584=VECTOR('',#24563,1000.);
#5585=VECTOR('',#24568,1000.);
#5586=CIRCLE('',#17790,22.5);
#5587=CIRCLE('',#17791,22.5);
#5588=CIRCLE('',#17793,25.);
#5589=CIRCLE('',#17794,25.);
#5590=CIRCLE('',#17798,22.5);
#5591=CIRCLE('',#17799,10.5);
#5592=CIRCLE('',#17801,10.5);
#5593=CIRCLE('',#17805,22.5);
#5594=CIRCLE('',#17808,22.5);
#5595=CIRCLE('',#17809,22.5);
#5596=CIRCLE('',#17811,10.5);
#5597=CIRCLE('',#17812,10.5);
#5598=CIRCLE('',#17814,25.);
#5599=CIRCLE('',#17815,25.);
#5600=CIRCLE('',#17820,22.5);
#5601=CIRCLE('',#17822,22.5);
#5602=CIRCLE('',#17829,22.5);
#5603=CIRCLE('',#17830,10.5);
#5604=CIRCLE('',#17832,22.5);
#5605=CIRCLE('',#17833,10.5);
#5606=CIRCLE('',#17836,22.5);
#5607=CIRCLE('',#17839,22.5);
#5608=CIRCLE('',#17845,22.5);
#5609=CIRCLE('',#17846,10.5);
#5610=CIRCLE('',#17848,22.5);
#5611=CIRCLE('',#17849,10.5);
#5612=CIRCLE('',#17852,22.5);
#5613=CIRCLE('',#17855,22.5);
#5614=CIRCLE('',#17859,10.);
#5615=CIRCLE('',#17860,10.);
#5616=CIRCLE('',#17862,8.);
#5617=CIRCLE('',#17866,8.);
#5618=CIRCLE('',#17869,8.);
#5619=CIRCLE('',#17870,8.);
#5620=CIRCLE('',#17872,10.);
#5621=CIRCLE('',#17873,10.);
#5622=CIRCLE('',#17883,8.);
#5623=CIRCLE('',#17884,8.);
#5624=CIRCLE('',#17887,8.);
#5625=CIRCLE('',#17890,8.);
#5626=CIRCLE('',#17893,2.6);
#5627=CIRCLE('',#17896,8.);
#5628=CIRCLE('',#17897,7.);
#5629=CIRCLE('',#17899,9.66270045344786);
#5630=CIRCLE('',#17900,9.66270045344786);
#5631=CIRCLE('',#17901,8.69677462715879);
#5632=CIRCLE('',#17903,8.);
#5633=CIRCLE('',#17905,10.);
#5634=CIRCLE('',#17935,4.29685191531251);
#5635=CIRCLE('',#17937,4.125);
#5636=CIRCLE('',#17939,4.125);
#5637=CIRCLE('',#17963,4.12499999999999);
#5638=CIRCLE('',#17965,4.15);
#5639=CIRCLE('',#17967,8.);
#5640=CIRCLE('',#17968,8.);
#5641=CIRCLE('',#17969,8.);
#5642=CIRCLE('',#17970,8.);
#5643=CIRCLE('',#17971,8.);
#5644=CIRCLE('',#17972,8.);
#5645=CIRCLE('',#17974,12.5);
#5646=CIRCLE('',#17975,1.00000000000001);
#5647=CIRCLE('',#17976,11.5);
#5648=CIRCLE('',#17978,12.5);
#5649=CIRCLE('',#17979,12.5);
#5650=CIRCLE('',#17980,12.5);
#5651=CIRCLE('',#17981,12.5);
#5652=CIRCLE('',#17982,12.5);
#5653=CIRCLE('',#17984,25.);
#5654=CIRCLE('',#17985,2.25);
#5655=CIRCLE('',#17986,22.75);
#5656=CIRCLE('',#17988,25.);
#5657=CIRCLE('',#17990,22.5);
#5658=CIRCLE('',#17991,22.5);
#5659=CIRCLE('',#18004,8.05);
#5660=CIRCLE('',#18005,8.05);
#5661=CIRCLE('',#18007,10.5);
#5662=CIRCLE('',#18008,10.5);
#5663=CIRCLE('',#18014,22.5);
#5664=CIRCLE('',#18015,22.5);
#5665=CIRCLE('',#18017,25.);
#5666=CIRCLE('',#18018,25.);
#5667=CIRCLE('',#18023,3.);
#5668=CIRCLE('',#18024,3.);
#5669=CIRCLE('',#18025,0.5);
#5670=CIRCLE('',#18026,2.5);
#5671=CIRCLE('',#18028,3.);
#5672=CIRCLE('',#18029,0.5);
#5673=CIRCLE('',#18030,2.5);
#5674=CIRCLE('',#18032,2.5);
#5675=CIRCLE('',#18038,8.);
#5676=CIRCLE('',#18039,2.);
#5677=CIRCLE('',#18040,10.);
#5678=CIRCLE('',#18042,10.);
#5679=CIRCLE('',#18044,9.5);
#5680=CIRCLE('',#18046,4.);
#5681=CIRCLE('',#18047,4.);
#5682=CIRCLE('',#18049,3.5);
#5683=CIRCLE('',#18051,9.);
#5684=CIRCLE('',#18052,5.);
#5685=CIRCLE('',#18054,5.);
#5686=CIRCLE('',#18060,9.11842675485531);
#5687=CIRCLE('',#18061,7.85653654166145);
#5688=CIRCLE('',#18063,1.);
#5689=CIRCLE('',#18064,1.);
#5690=CIRCLE('',#18065,0.999999999999999);
#5691=CIRCLE('',#18067,6.);
#5692=CIRCLE('',#18068,0.999999999999998);
#5693=CIRCLE('',#18069,7.62222222222222);
#5694=CIRCLE('',#18071,6.);
#5695=CIRCLE('',#18073,6.57777777777778);
#5696=CIRCLE('',#18075,9.25);
#5697=CIRCLE('',#18076,9.25);
#5698=CIRCLE('',#18077,6.);
#5699=CIRCLE('',#18078,9.25);
#5700=CIRCLE('',#18080,12.25);
#5701=CIRCLE('',#18081,12.25);
#5702=CIRCLE('',#18084,10.3623383247004);
#5703=CIRCLE('',#18085,10.3623383247004);
#5704=CIRCLE('',#18087,6.);
#5705=CIRCLE('',#18090,9.25);
#5706=CIRCLE('',#18092,9.25);
#5707=CIRCLE('',#18095,1.);
#5708=CIRCLE('',#18096,1.);
#5709=CIRCLE('',#18098,1.);
#5710=CIRCLE('',#18099,1.);
#5711=CIRCLE('',#18101,9.51643315533714);
#5712=CIRCLE('',#18103,9.51643315533713);
#5713=CIRCLE('',#18104,1.);
#5714=CIRCLE('',#18105,1.);
#5715=CIRCLE('',#18106,1.);
#5716=CIRCLE('',#18108,1.);
#5717=CIRCLE('',#18110,1.);
#5718=CIRCLE('',#18112,1.);
#5719=CIRCLE('',#18114,1.);
#5720=CIRCLE('',#18116,1.);
#5721=CIRCLE('',#18117,1.);
#5722=CIRCLE('',#18119,1.);
#5723=CIRCLE('',#18122,1.);
#5724=CIRCLE('',#18124,1.);
#5725=CIRCLE('',#18125,1.);
#5726=CIRCLE('',#18126,1.);
#5727=CIRCLE('',#18129,15.);
#5728=CIRCLE('',#18130,11.1803398874989);
#5729=CIRCLE('',#18131,10.);
#5730=CIRCLE('',#18132,11.1803398874989);
#5731=CIRCLE('',#18134,6.);
#5732=CIRCLE('',#18135,6.);
#5733=CIRCLE('',#18137,11.1803398874989);
#5734=CIRCLE('',#18138,10.);
#5735=CIRCLE('',#18139,11.1803398874989);
#5736=CIRCLE('',#18141,6.);
#5737=CIRCLE('',#18143,6.);
#5738=CIRCLE('',#18145,5.5);
#5739=CIRCLE('',#18151,5.5);
#5740=CIRCLE('',#18152,6.41621047834285);
#5741=CIRCLE('',#18153,6.41621047834285);
#5742=CIRCLE('',#18155,5.5);
#5743=CIRCLE('',#18156,5.5);
#5744=CIRCLE('',#18157,5.5);
#5745=CIRCLE('',#18159,6.04796058042142);
#5746=CIRCLE('',#18160,4.94835215326525);
#5747=CIRCLE('',#18162,1.23243402184158);
#5748=CIRCLE('',#18163,6.53216674526026);
#5749=CIRCLE('',#18164,1.23243402184158);
#5750=CIRCLE('',#18165,4.25614904904292);
#5751=CIRCLE('',#18167,5.5);
#5752=CIRCLE('',#18168,4.);
#5753=CIRCLE('',#18169,5.5);
#5754=CIRCLE('',#18171,4.);
#5755=CIRCLE('',#18173,6.72023753462643);
#5756=CIRCLE('',#18174,6.72023753462643);
#5757=CIRCLE('',#18176,5.7816585169653);
#5758=CIRCLE('',#18177,6.41621047834285);
#5759=CIRCLE('',#18178,7.70789157434132);
#5760=CIRCLE('',#18179,6.41621047834285);
#5761=CIRCLE('',#18180,7.70789157434132);
#5762=CIRCLE('',#18181,5.7816585169653);
#5763=CIRCLE('',#18184,5.40661052483917);
#5764=CIRCLE('',#18186,5.40661052483917);
#5765=CIRCLE('',#18188,0.5);
#5766=CIRCLE('',#18190,0.5);
#5767=CIRCLE('',#18191,0.5);
#5768=CIRCLE('',#18195,0.5);
#5769=CIRCLE('',#18198,15.);
#5770=CIRCLE('',#18199,11.1803398874989);
#5771=CIRCLE('',#18200,10.);
#5772=CIRCLE('',#18201,11.1803398874989);
#5773=CIRCLE('',#18203,6.);
#5774=CIRCLE('',#18204,6.);
#5775=CIRCLE('',#18206,11.1803398874989);
#5776=CIRCLE('',#18207,10.);
#5777=CIRCLE('',#18208,11.1803398874989);
#5778=CIRCLE('',#18210,4.);
#5779=CIRCLE('',#18212,4.);
#5780=CIRCLE('',#18214,3.5);
#5781=CIRCLE('',#18220,12.5);
#5782=CIRCLE('',#18221,12.5);
#5783=CIRCLE('',#18222,2.);
#5784=CIRCLE('',#18223,10.5);
#5785=CIRCLE('',#18225,5.);
#5786=CIRCLE('',#18226,4.25);
#5787=CIRCLE('',#18228,5.);
#5788=CIRCLE('',#18229,5.);
#5789=CIRCLE('',#18231,4.25);
#5790=CIRCLE('',#18232,4.25);
#5791=CIRCLE('',#18234,4.25);
#5792=CIRCLE('',#18236,6.);
#5793=CIRCLE('',#18237,6.);
#5794=CIRCLE('',#18239,12.5);
#5795=CIRCLE('',#18246,6.00000000000022);
#5796=CIRCLE('',#18247,2.);
#5797=CIRCLE('',#18248,8.00000000000022);
#5798=CIRCLE('',#18249,2.);
#5799=CIRCLE('',#18251,2.);
#5800=CIRCLE('',#18252,2.);
#5801=CIRCLE('',#18254,6.);
#5802=CIRCLE('',#18255,2.);
#5803=CIRCLE('',#18256,8.);
#5804=CIRCLE('',#18257,2.);
#5805=CIRCLE('',#18259,6.00000000000095);
#5806=CIRCLE('',#18260,2.);
#5807=CIRCLE('',#18261,8.00000000000095);
#5808=CIRCLE('',#18262,2.);
#5809=CIRCLE('',#18264,2.);
#5810=CIRCLE('',#18265,2.);
#5811=CIRCLE('',#18267,6.00000000000152);
#5812=CIRCLE('',#18268,2.);
#5813=CIRCLE('',#18269,8.00000000000152);
#5814=CIRCLE('',#18270,2.);
#5815=CIRCLE('',#18272,2.);
#5816=CIRCLE('',#18273,2.);
#5817=CIRCLE('',#18275,6.00000000000143);
#5818=CIRCLE('',#18276,2.);
#5819=CIRCLE('',#18277,8.00000000000143);
#5820=CIRCLE('',#18278,2.);
#5821=CIRCLE('',#18280,6.00000000000081);
#5822=CIRCLE('',#18281,2.);
#5823=CIRCLE('',#18282,8.00000000000082);
#5824=CIRCLE('',#18283,2.);
#5825=CIRCLE('',#18285,2.);
#5826=CIRCLE('',#18286,2.);
#5827=CIRCLE('',#18288,6.00000000000143);
#5828=CIRCLE('',#18290,6.00000000000152);
#5829=CIRCLE('',#18292,6.00000000000095);
#5830=CIRCLE('',#18294,5.);
#5831=CIRCLE('',#18295,5.);
#5832=CIRCLE('',#18297,12.5);
#5833=CIRCLE('',#18298,12.5);
#5834=CIRCLE('',#18300,25.);
#5835=CIRCLE('',#18301,25.);
#5836=CIRCLE('',#18303,25.);
#5837=CIRCLE('',#18304,25.);
#5838=CIRCLE('',#18306,25.);
#5839=CIRCLE('',#18307,25.);
#5840=CIRCLE('',#18309,25.);
#5841=CIRCLE('',#18310,25.);
#5842=CIRCLE('',#18312,25.);
#5843=CIRCLE('',#18313,25.);
#5844=CIRCLE('',#18315,23.);
#5845=CIRCLE('',#18316,2.);
#5846=CIRCLE('',#18317,2.);
#5847=CIRCLE('',#18319,23.);
#5848=CIRCLE('',#18320,2.);
#5849=CIRCLE('',#18321,2.);
#5850=CIRCLE('',#18323,2.);
#5851=CIRCLE('',#18324,23.);
#5852=CIRCLE('',#18325,2.);
#5853=CIRCLE('',#18327,2.);
#5854=CIRCLE('',#18328,23.);
#5855=CIRCLE('',#18329,2.);
#5856=CIRCLE('',#18331,25.);
#5857=CIRCLE('',#18332,2.);
#5858=CIRCLE('',#18333,23.);
#5859=CIRCLE('',#18334,2.);
#5860=CIRCLE('',#18336,2.);
#5861=CIRCLE('',#18337,23.);
#5862=CIRCLE('',#18338,2.);
#5863=CIRCLE('',#18340,2.);
#5864=CIRCLE('',#18341,23.);
#5865=CIRCLE('',#18342,2.);
#5866=CIRCLE('',#18344,23.);
#5867=CIRCLE('',#18345,2.);
#5868=CIRCLE('',#18346,2.);
#5869=CIRCLE('',#18348,23.);
#5870=CIRCLE('',#18349,2.);
#5871=CIRCLE('',#18350,2.);
#5872=CIRCLE('',#18352,23.);
#5873=CIRCLE('',#18353,2.);
#5874=CIRCLE('',#18354,25.);
#5875=CIRCLE('',#18355,2.);
#5876=CIRCLE('',#18357,8.00000000000082);
#5877=CIRCLE('',#18358,8.);
#5878=CIRCLE('',#18359,8.00000000000022);
#5879=CIRCLE('',#18360,23.);
#5880=CIRCLE('',#18363,8.00000000000143);
#5881=CIRCLE('',#18364,8.00000000000151);
#5882=CIRCLE('',#18365,23.);
#5883=CIRCLE('',#18366,8.00000000000095);
#5884=CIRCLE('',#18370,2.);
#5885=CIRCLE('',#18371,2.);
#5886=CIRCLE('',#18373,2.);
#5887=CIRCLE('',#18374,2.);
#5888=CIRCLE('',#18376,6.00000000000022);
#5889=CIRCLE('',#18378,6.00000000000081);
#5890=CIRCLE('',#18380,6.);
#5891=CIRCLE('',#18382,2.);
#5892=CIRCLE('',#18385,2.);
#5893=CIRCLE('',#18387,2.);
#5894=CIRCLE('',#18389,2.);
#5895=CIRCLE('',#18392,2.);
#5896=CIRCLE('',#18393,2.);
#5897=CIRCLE('',#18396,2.);
#5898=CIRCLE('',#18398,2.);
#5899=CIRCLE('',#18402,2.);
#5900=CIRCLE('',#18403,2.);
#5901=CIRCLE('',#18406,2.);
#5902=CIRCLE('',#18408,2.);
#5903=CIRCLE('',#18412,2.);
#5904=CIRCLE('',#18413,2.);
#5905=CIRCLE('',#18415,2.);
#5906=CIRCLE('',#18417,2.);
#5907=CIRCLE('',#18419,2.);
#5908=CIRCLE('',#18421,2.);
#5909=CIRCLE('',#18426,2.);
#5910=CIRCLE('',#18428,2.);
#5911=CIRCLE('',#18430,2.);
#5912=CIRCLE('',#18432,2.);
#5913=CIRCLE('',#18435,2.);
#5914=CIRCLE('',#18437,2.);
#5915=CIRCLE('',#18439,2.);
#5916=CIRCLE('',#18441,2.);
#5917=CIRCLE('',#18443,2.);
#5918=CIRCLE('',#18445,2.);
#5919=CIRCLE('',#18449,2.);
#5920=CIRCLE('',#18450,2.3);
#5921=CIRCLE('',#18452,1.5);
#5922=CIRCLE('',#18453,1.5);
#5923=CIRCLE('',#18454,1.80000000000002);
#5924=CIRCLE('',#18456,2.);
#5925=CIRCLE('',#18457,2.);
#5926=CIRCLE('',#18458,2.3);
#5927=CIRCLE('',#18460,1.2);
#5928=CIRCLE('',#18461,1.50000000000002);
#5929=CIRCLE('',#18463,3.2);
#5930=CIRCLE('',#18464,3.49999999999998);
#5931=CIRCLE('',#18466,1.2);
#5932=CIRCLE('',#18467,1.2);
#5933=CIRCLE('',#18468,1.50000000000001);
#5934=CIRCLE('',#18470,2.);
#5935=CIRCLE('',#18471,2.);
#5936=CIRCLE('',#18472,2.3);
#5937=CIRCLE('',#18474,2.);
#5938=CIRCLE('',#18475,2.29999999999998);
#5939=CIRCLE('',#18477,1.5);
#5940=CIRCLE('',#18478,1.8);
#5941=CIRCLE('',#18480,3.2);
#5942=CIRCLE('',#18481,3.50000000000001);
#5943=CIRCLE('',#18483,2.);
#5944=CIRCLE('',#18484,2.);
#5945=CIRCLE('',#18486,2.);
#5946=CIRCLE('',#18494,4.3);
#5947=CIRCLE('',#18495,4.3);
#5948=CIRCLE('',#18498,4.29999999999998);
#5949=CIRCLE('',#18499,4.29999999999999);
#5950=CIRCLE('',#18503,3.3);
#5951=CIRCLE('',#18505,3.3);
#5952=CIRCLE('',#18507,4.);
#5953=CIRCLE('',#18508,4.);
#5954=CIRCLE('',#18512,4.);
#5955=CIRCLE('',#18513,4.);
#5956=CIRCLE('',#18521,3.);
#5957=CIRCLE('',#18526,3.);
#5958=CIRCLE('',#18528,3.);
#5959=CIRCLE('',#18531,3.);
#5960=CIRCLE('',#18533,0.300000000000002);
#5961=CIRCLE('',#18538,0.300000000000002);
#5962=CIRCLE('',#18539,0.300000000000002);
#5963=CIRCLE('',#18541,0.300000000000002);
#5964=CIRCLE('',#18543,0.300000000000002);
#5965=CIRCLE('',#18546,0.300000000000002);
#5966=CIRCLE('',#18548,0.300000000000002);
#5967=CIRCLE('',#18549,0.300000000000002);
#5968=CIRCLE('',#18553,0.300000000000002);
#5969=CIRCLE('',#18554,0.300000000000002);
#5970=CIRCLE('',#18556,0.300000000000002);
#5971=CIRCLE('',#18558,0.300000000000002);
#5972=CIRCLE('',#18560,0.300000000000002);
#5973=CIRCLE('',#18562,0.300000000000002);
#5974=CIRCLE('',#18564,0.300000000000002);
#5975=CIRCLE('',#18566,0.300000000000002);
#5976=CIRCLE('',#18568,0.300000000000002);
#5977=CIRCLE('',#18572,0.300000000000002);
#5978=CIRCLE('',#18574,0.300000000000002);
#5979=CIRCLE('',#18578,0.300000000000002);
#5980=CIRCLE('',#18581,0.300000000000002);
#5981=CIRCLE('',#18591,0.300000000000002);
#5982=CIRCLE('',#18598,1.1);
#5983=CIRCLE('',#18599,0.1);
#5984=CIRCLE('',#18600,1.2);
#5985=CIRCLE('',#18601,1.2);
#5986=CIRCLE('',#18603,1.2);
#5987=CIRCLE('',#18604,1.2);
#5988=CIRCLE('',#18605,0.1);
#5989=CIRCLE('',#18606,1.1);
#5990=CIRCLE('',#18611,2.5);
#5991=CIRCLE('',#18612,2.5);
#5992=CIRCLE('',#18614,3.);
#5993=CIRCLE('',#18615,3.);
#5994=CIRCLE('',#18616,3.);
#5995=CIRCLE('',#18617,3.);
#5996=CIRCLE('',#18619,4.25);
#5997=CIRCLE('',#18620,4.25);
#5998=CIRCLE('',#18622,1.2);
#5999=CIRCLE('',#18623,1.2);
#6000=CIRCLE('',#18625,1.2);
#6001=CIRCLE('',#18626,1.2);
#6002=CIRCLE('',#18628,2.);
#6003=CIRCLE('',#18629,2.);
#6004=CIRCLE('',#18632,1.5);
#6005=CIRCLE('',#18633,1.5);
#6006=CIRCLE('',#18637,1.5);
#6007=CIRCLE('',#18641,1.5);
#6008=CIRCLE('',#18651,2.5);
#6009=CIRCLE('',#18652,2.5);
#6010=CIRCLE('',#18654,5.5);
#6011=CIRCLE('',#18657,2.5);
#6012=CIRCLE('',#18658,0.5);
#6013=CIRCLE('',#18659,2.);
#6014=CIRCLE('',#18661,1.99814869273444);
#6015=CIRCLE('',#18662,1.99814869273444);
#6016=CIRCLE('',#18663,1.61);
#6017=CIRCLE('',#18665,2.);
#6018=CIRCLE('',#18666,2.);
#6019=CIRCLE('',#18667,1.61);
#6020=CIRCLE('',#18668,1.61);
#6021=CIRCLE('',#18671,2.);
#6022=CIRCLE('',#18672,2.);
#6023=CIRCLE('',#18674,2.);
#6024=CIRCLE('',#18675,2.);
#6025=CIRCLE('',#18676,1.61);
#6026=CIRCLE('',#18677,1.61);
#6027=CIRCLE('',#18680,2.);
#6028=CIRCLE('',#18681,2.);
#6029=CIRCLE('',#18683,2.);
#6030=CIRCLE('',#18684,2.);
#6031=CIRCLE('',#18685,1.61);
#6032=CIRCLE('',#18686,1.61);
#6033=CIRCLE('',#18689,2.);
#6034=CIRCLE('',#18690,2.);
#6035=CIRCLE('',#18692,2.);
#6036=CIRCLE('',#18693,2.);
#6037=CIRCLE('',#18694,1.61);
#6038=CIRCLE('',#18695,1.61);
#6039=CIRCLE('',#18698,2.);
#6040=CIRCLE('',#18699,2.);
#6041=CIRCLE('',#18701,2.);
#6042=CIRCLE('',#18702,2.);
#6043=CIRCLE('',#18703,1.61);
#6044=CIRCLE('',#18704,1.61);
#6045=CIRCLE('',#18707,2.);
#6046=CIRCLE('',#18708,2.);
#6047=CIRCLE('',#18710,2.);
#6048=CIRCLE('',#18711,2.);
#6049=CIRCLE('',#18712,1.61);
#6050=CIRCLE('',#18713,1.61);
#6051=CIRCLE('',#18716,2.);
#6052=CIRCLE('',#18717,2.);
#6053=CIRCLE('',#18719,2.);
#6054=CIRCLE('',#18720,2.);
#6055=CIRCLE('',#18721,1.61);
#6056=CIRCLE('',#18722,1.61);
#6057=CIRCLE('',#18725,2.);
#6058=CIRCLE('',#18726,2.);
#6059=CIRCLE('',#18728,2.);
#6060=CIRCLE('',#18729,2.);
#6061=CIRCLE('',#18730,1.61);
#6062=CIRCLE('',#18731,1.61);
#6063=CIRCLE('',#18734,2.);
#6064=CIRCLE('',#18735,2.);
#6065=CIRCLE('',#18737,2.);
#6066=CIRCLE('',#18738,2.);
#6067=CIRCLE('',#18739,1.61);
#6068=CIRCLE('',#18740,1.61);
#6069=CIRCLE('',#18743,2.);
#6070=CIRCLE('',#18744,2.);
#6071=CIRCLE('',#18746,2.);
#6072=CIRCLE('',#18747,2.);
#6073=CIRCLE('',#18748,1.61);
#6074=CIRCLE('',#18749,1.61);
#6075=CIRCLE('',#18752,2.);
#6076=CIRCLE('',#18753,2.);
#6077=CIRCLE('',#18755,2.);
#6078=CIRCLE('',#18756,2.);
#6079=CIRCLE('',#18757,1.61);
#6080=CIRCLE('',#18758,1.61);
#6081=CIRCLE('',#18761,2.);
#6082=CIRCLE('',#18762,2.);
#6083=CIRCLE('',#18764,2.);
#6084=CIRCLE('',#18765,2.);
#6085=CIRCLE('',#18766,1.61);
#6086=CIRCLE('',#18767,1.61);
#6087=CIRCLE('',#18770,2.);
#6088=CIRCLE('',#18771,2.);
#6089=CIRCLE('',#18773,2.);
#6090=CIRCLE('',#18774,2.);
#6091=CIRCLE('',#18775,1.61);
#6092=CIRCLE('',#18776,1.61);
#6093=CIRCLE('',#18779,2.);
#6094=CIRCLE('',#18780,2.);
#6095=CIRCLE('',#18782,2.);
#6096=CIRCLE('',#18783,2.);
#6097=CIRCLE('',#18784,1.61);
#6098=CIRCLE('',#18785,1.61);
#6099=CIRCLE('',#18788,2.);
#6100=CIRCLE('',#18789,2.);
#6101=CIRCLE('',#18791,2.);
#6102=CIRCLE('',#18792,2.);
#6103=CIRCLE('',#18793,1.61);
#6104=CIRCLE('',#18794,1.61);
#6105=CIRCLE('',#18797,8.175);
#6106=CIRCLE('',#18798,8.175);
#6107=CIRCLE('',#18799,8.175);
#6108=CIRCLE('',#18800,8.175);
#6109=CIRCLE('',#18801,8.175);
#6110=CIRCLE('',#18802,8.175);
#6111=CIRCLE('',#18803,8.175);
#6112=CIRCLE('',#18804,8.175);
#6113=CIRCLE('',#18805,8.175);
#6114=CIRCLE('',#18806,8.175);
#6115=CIRCLE('',#18807,8.175);
#6116=CIRCLE('',#18808,8.175);
#6117=CIRCLE('',#18809,8.175);
#6118=CIRCLE('',#18810,8.175);
#6119=CIRCLE('',#18811,8.175);
#6120=CIRCLE('',#18812,8.175);
#6121=CIRCLE('',#18813,8.175);
#6122=CIRCLE('',#18814,8.175);
#6123=CIRCLE('',#18815,8.175);
#6124=CIRCLE('',#18816,8.175);
#6125=CIRCLE('',#18817,8.175);
#6126=CIRCLE('',#18818,8.175);
#6127=CIRCLE('',#18819,8.175);
#6128=CIRCLE('',#18820,8.175);
#6129=CIRCLE('',#18821,8.175);
#6130=CIRCLE('',#18822,8.175);
#6131=CIRCLE('',#18823,8.175);
#6132=CIRCLE('',#18824,8.175);
#6133=CIRCLE('',#18825,8.175);
#6134=CIRCLE('',#18826,8.175);
#6135=CIRCLE('',#18827,8.175);
#6136=CIRCLE('',#18828,8.175);
#6137=CIRCLE('',#18829,8.175);
#6138=CIRCLE('',#18830,8.175);
#6139=CIRCLE('',#18831,8.175);
#6140=CIRCLE('',#18832,8.175);
#6141=CIRCLE('',#18833,8.175);
#6142=CIRCLE('',#18834,8.175);
#6143=CIRCLE('',#18835,8.175);
#6144=CIRCLE('',#18836,7.775);
#6145=CIRCLE('',#18837,8.175);
#6146=CIRCLE('',#18838,8.175);
#6147=CIRCLE('',#18839,8.175);
#6148=CIRCLE('',#18840,8.175);
#6149=CIRCLE('',#18841,8.175);
#6150=CIRCLE('',#18842,8.175);
#6151=CIRCLE('',#18843,8.175);
#6152=CIRCLE('',#18844,8.175);
#6153=CIRCLE('',#18845,8.175);
#6154=CIRCLE('',#18846,8.175);
#6155=CIRCLE('',#18847,8.175);
#6156=CIRCLE('',#18848,8.175);
#6157=CIRCLE('',#18849,8.175);
#6158=CIRCLE('',#18850,8.175);
#6159=CIRCLE('',#18851,8.175);
#6160=CIRCLE('',#18852,8.175);
#6161=CIRCLE('',#18853,8.175);
#6162=CIRCLE('',#18854,8.175);
#6163=CIRCLE('',#18855,8.175);
#6164=CIRCLE('',#18856,8.175);
#6165=CIRCLE('',#18857,8.175);
#6166=CIRCLE('',#18858,8.175);
#6167=CIRCLE('',#18859,8.175);
#6168=CIRCLE('',#18860,8.175);
#6169=CIRCLE('',#18861,8.175);
#6170=CIRCLE('',#18862,8.175);
#6171=CIRCLE('',#18863,8.175);
#6172=CIRCLE('',#18864,8.175);
#6173=CIRCLE('',#18865,8.175);
#6174=CIRCLE('',#18866,8.175);
#6175=CIRCLE('',#18867,8.175);
#6176=CIRCLE('',#18868,8.175);
#6177=CIRCLE('',#18869,8.175);
#6178=CIRCLE('',#18870,8.175);
#6179=CIRCLE('',#18871,8.175);
#6180=CIRCLE('',#18872,8.175);
#6181=CIRCLE('',#18873,8.175);
#6182=CIRCLE('',#18874,8.175);
#6183=CIRCLE('',#18876,8.175);
#6184=CIRCLE('',#18877,8.175);
#6185=CIRCLE('',#18878,8.175);
#6186=CIRCLE('',#18879,8.175);
#6187=CIRCLE('',#18880,8.175);
#6188=CIRCLE('',#18881,8.175);
#6189=CIRCLE('',#18882,8.175);
#6190=CIRCLE('',#18883,8.175);
#6191=CIRCLE('',#18884,8.175);
#6192=CIRCLE('',#18885,8.175);
#6193=CIRCLE('',#18886,8.175);
#6194=CIRCLE('',#18887,8.175);
#6195=CIRCLE('',#18888,8.175);
#6196=CIRCLE('',#18889,8.175);
#6197=CIRCLE('',#18890,8.175);
#6198=CIRCLE('',#18891,8.175);
#6199=CIRCLE('',#18892,8.175);
#6200=CIRCLE('',#18893,8.175);
#6201=CIRCLE('',#18894,8.175);
#6202=CIRCLE('',#18895,8.175);
#6203=CIRCLE('',#18896,8.175);
#6204=CIRCLE('',#18897,8.175);
#6205=CIRCLE('',#18898,8.175);
#6206=CIRCLE('',#18899,8.175);
#6207=CIRCLE('',#18900,8.175);
#6208=CIRCLE('',#18901,8.175);
#6209=CIRCLE('',#18902,8.175);
#6210=CIRCLE('',#18903,8.175);
#6211=CIRCLE('',#18904,8.175);
#6212=CIRCLE('',#18905,8.175);
#6213=CIRCLE('',#18906,8.175);
#6214=CIRCLE('',#18907,8.175);
#6215=CIRCLE('',#18908,8.175);
#6216=CIRCLE('',#18909,8.175);
#6217=CIRCLE('',#18910,8.175);
#6218=CIRCLE('',#18911,8.175);
#6219=CIRCLE('',#18912,8.175);
#6220=CIRCLE('',#18913,8.175);
#6221=CIRCLE('',#18914,8.175);
#6222=CIRCLE('',#18915,7.775);
#6223=CIRCLE('',#18916,8.175);
#6224=CIRCLE('',#18917,8.175);
#6225=CIRCLE('',#18918,8.175);
#6226=CIRCLE('',#18919,8.175);
#6227=CIRCLE('',#18920,8.175);
#6228=CIRCLE('',#18921,8.175);
#6229=CIRCLE('',#18922,8.175);
#6230=CIRCLE('',#18923,8.175);
#6231=CIRCLE('',#18924,8.175);
#6232=CIRCLE('',#18925,8.175);
#6233=CIRCLE('',#18926,8.175);
#6234=CIRCLE('',#18927,8.175);
#6235=CIRCLE('',#18928,8.175);
#6236=CIRCLE('',#18929,8.175);
#6237=CIRCLE('',#18930,8.175);
#6238=CIRCLE('',#18931,8.175);
#6239=CIRCLE('',#18932,8.175);
#6240=CIRCLE('',#18933,8.175);
#6241=CIRCLE('',#18934,8.175);
#6242=CIRCLE('',#18935,8.175);
#6243=CIRCLE('',#18936,8.175);
#6244=CIRCLE('',#18937,8.175);
#6245=CIRCLE('',#18938,8.175);
#6246=CIRCLE('',#18939,8.175);
#6247=CIRCLE('',#18940,8.175);
#6248=CIRCLE('',#18941,8.175);
#6249=CIRCLE('',#18942,8.175);
#6250=CIRCLE('',#18943,8.175);
#6251=CIRCLE('',#18944,8.175);
#6252=CIRCLE('',#18945,8.175);
#6253=CIRCLE('',#18946,8.175);
#6254=CIRCLE('',#18947,8.175);
#6255=CIRCLE('',#18948,8.175);
#6256=CIRCLE('',#18949,8.175);
#6257=CIRCLE('',#18950,8.175);
#6258=CIRCLE('',#18951,8.175);
#6259=CIRCLE('',#18952,8.175);
#6260=CIRCLE('',#18953,8.175);
#6261=CIRCLE('',#19190,2.69531878777687);
#6262=CIRCLE('',#19191,1.81782234903766);
#6263=CIRCLE('',#19192,2.69531878777687);
#6264=CIRCLE('',#19193,0.9);
#6265=CIRCLE('',#19194,2.71439757732023);
#6266=CIRCLE('',#19195,2.71439757732023);
#6267=CIRCLE('',#19196,2.69531878777687);
#6268=CIRCLE('',#19197,1.81782234903766);
#6269=CIRCLE('',#19199,2.8);
#6270=CIRCLE('',#19201,1.5);
#6271=CIRCLE('',#19202,1.5);
#6272=CIRCLE('',#19211,4.5);
#6273=CIRCLE('',#19212,0.5);
#6274=CIRCLE('',#19213,4.);
#6275=CIRCLE('',#19215,1.99909277054204);
#6276=CIRCLE('',#19216,1.99909277054204);
#6277=CIRCLE('',#19217,1.61);
#6278=CIRCLE('',#19219,2.);
#6279=CIRCLE('',#19220,2.);
#6280=CIRCLE('',#19221,1.61);
#6281=CIRCLE('',#19222,1.61);
#6282=CIRCLE('',#19225,2.);
#6283=CIRCLE('',#19226,2.);
#6284=CIRCLE('',#19228,2.);
#6285=CIRCLE('',#19229,2.);
#6286=CIRCLE('',#19230,1.61);
#6287=CIRCLE('',#19231,1.61);
#6288=CIRCLE('',#19234,2.);
#6289=CIRCLE('',#19235,2.);
#6290=CIRCLE('',#19237,2.);
#6291=CIRCLE('',#19238,2.);
#6292=CIRCLE('',#19239,1.61);
#6293=CIRCLE('',#19240,1.61);
#6294=CIRCLE('',#19243,2.);
#6295=CIRCLE('',#19244,2.);
#6296=CIRCLE('',#19246,2.);
#6297=CIRCLE('',#19247,2.);
#6298=CIRCLE('',#19248,1.61);
#6299=CIRCLE('',#19249,1.61);
#6300=CIRCLE('',#19252,2.);
#6301=CIRCLE('',#19253,2.);
#6302=CIRCLE('',#19255,2.);
#6303=CIRCLE('',#19256,2.);
#6304=CIRCLE('',#19257,1.61);
#6305=CIRCLE('',#19258,1.61);
#6306=CIRCLE('',#19261,2.);
#6307=CIRCLE('',#19262,2.);
#6308=CIRCLE('',#19264,2.);
#6309=CIRCLE('',#19265,2.);
#6310=CIRCLE('',#19266,1.61);
#6311=CIRCLE('',#19267,1.61);
#6312=CIRCLE('',#19270,2.);
#6313=CIRCLE('',#19271,2.);
#6314=CIRCLE('',#19273,2.);
#6315=CIRCLE('',#19274,2.);
#6316=CIRCLE('',#19275,1.61);
#6317=CIRCLE('',#19276,1.61);
#6318=CIRCLE('',#19279,2.);
#6319=CIRCLE('',#19280,2.);
#6320=CIRCLE('',#19282,2.);
#6321=CIRCLE('',#19283,2.);
#6322=CIRCLE('',#19284,1.61);
#6323=CIRCLE('',#19285,1.61);
#6324=CIRCLE('',#19288,2.);
#6325=CIRCLE('',#19289,2.);
#6326=CIRCLE('',#19291,2.);
#6327=CIRCLE('',#19292,2.);
#6328=CIRCLE('',#19293,1.61);
#6329=CIRCLE('',#19294,1.61);
#6330=CIRCLE('',#19297,2.);
#6331=CIRCLE('',#19298,2.);
#6332=CIRCLE('',#19300,2.);
#6333=CIRCLE('',#19301,2.);
#6334=CIRCLE('',#19302,1.61);
#6335=CIRCLE('',#19303,1.61);
#6336=CIRCLE('',#19306,2.);
#6337=CIRCLE('',#19307,2.);
#6338=CIRCLE('',#19309,2.);
#6339=CIRCLE('',#19310,2.);
#6340=CIRCLE('',#19311,1.61);
#6341=CIRCLE('',#19312,1.61);
#6342=CIRCLE('',#19315,2.);
#6343=CIRCLE('',#19316,2.);
#6344=CIRCLE('',#19318,2.);
#6345=CIRCLE('',#19319,2.);
#6346=CIRCLE('',#19320,1.61);
#6347=CIRCLE('',#19321,1.61);
#6348=CIRCLE('',#19324,2.);
#6349=CIRCLE('',#19325,2.);
#6350=CIRCLE('',#19327,2.);
#6351=CIRCLE('',#19328,2.);
#6352=CIRCLE('',#19329,1.61);
#6353=CIRCLE('',#19330,1.61);
#6354=CIRCLE('',#19333,4.);
#6355=CIRCLE('',#19335,8.175);
#6356=CIRCLE('',#19336,8.175);
#6357=CIRCLE('',#19337,8.175);
#6358=CIRCLE('',#19338,8.175);
#6359=CIRCLE('',#19339,8.175);
#6360=CIRCLE('',#19340,8.175);
#6361=CIRCLE('',#19341,8.175);
#6362=CIRCLE('',#19342,8.175);
#6363=CIRCLE('',#19343,8.175);
#6364=CIRCLE('',#19344,8.175);
#6365=CIRCLE('',#19345,8.175);
#6366=CIRCLE('',#19346,8.175);
#6367=CIRCLE('',#19347,8.175);
#6368=CIRCLE('',#19348,8.175);
#6369=CIRCLE('',#19349,8.175);
#6370=CIRCLE('',#19350,8.175);
#6371=CIRCLE('',#19351,8.175);
#6372=CIRCLE('',#19352,8.175);
#6373=CIRCLE('',#19353,8.175);
#6374=CIRCLE('',#19354,8.175);
#6375=CIRCLE('',#19355,8.175);
#6376=CIRCLE('',#19356,8.175);
#6377=CIRCLE('',#19357,8.175);
#6378=CIRCLE('',#19358,8.175);
#6379=CIRCLE('',#19359,8.175);
#6380=CIRCLE('',#19360,8.175);
#6381=CIRCLE('',#19361,8.175);
#6382=CIRCLE('',#19362,8.175);
#6383=CIRCLE('',#19363,8.175);
#6384=CIRCLE('',#19364,8.175);
#6385=CIRCLE('',#19365,8.175);
#6386=CIRCLE('',#19366,8.175);
#6387=CIRCLE('',#19367,8.175);
#6388=CIRCLE('',#19368,8.175);
#6389=CIRCLE('',#19369,8.175);
#6390=CIRCLE('',#19370,8.175);
#6391=CIRCLE('',#19371,8.175);
#6392=CIRCLE('',#19372,8.175);
#6393=CIRCLE('',#19373,8.175);
#6394=CIRCLE('',#19374,7.775);
#6395=CIRCLE('',#19375,8.175);
#6396=CIRCLE('',#19376,8.175);
#6397=CIRCLE('',#19377,8.175);
#6398=CIRCLE('',#19378,8.175);
#6399=CIRCLE('',#19379,8.175);
#6400=CIRCLE('',#19380,8.175);
#6401=CIRCLE('',#19381,8.175);
#6402=CIRCLE('',#19382,8.175);
#6403=CIRCLE('',#19383,8.175);
#6404=CIRCLE('',#19384,8.175);
#6405=CIRCLE('',#19385,8.175);
#6406=CIRCLE('',#19386,8.175);
#6407=CIRCLE('',#19387,8.175);
#6408=CIRCLE('',#19388,8.175);
#6409=CIRCLE('',#19389,8.175);
#6410=CIRCLE('',#19390,8.175);
#6411=CIRCLE('',#19391,8.175);
#6412=CIRCLE('',#19392,8.175);
#6413=CIRCLE('',#19393,8.175);
#6414=CIRCLE('',#19394,8.175);
#6415=CIRCLE('',#19395,8.175);
#6416=CIRCLE('',#19396,8.175);
#6417=CIRCLE('',#19397,8.175);
#6418=CIRCLE('',#19398,8.175);
#6419=CIRCLE('',#19399,8.175);
#6420=CIRCLE('',#19400,8.175);
#6421=CIRCLE('',#19401,8.175);
#6422=CIRCLE('',#19402,8.175);
#6423=CIRCLE('',#19403,8.175);
#6424=CIRCLE('',#19404,8.175);
#6425=CIRCLE('',#19405,8.175);
#6426=CIRCLE('',#19406,8.175);
#6427=CIRCLE('',#19407,8.175);
#6428=CIRCLE('',#19408,8.175);
#6429=CIRCLE('',#19409,8.175);
#6430=CIRCLE('',#19410,8.175);
#6431=CIRCLE('',#19411,8.175);
#6432=CIRCLE('',#19412,8.175);
#6433=CIRCLE('',#19414,8.175);
#6434=CIRCLE('',#19415,8.175);
#6435=CIRCLE('',#19416,8.175);
#6436=CIRCLE('',#19417,8.175);
#6437=CIRCLE('',#19418,8.175);
#6438=CIRCLE('',#19419,8.175);
#6439=CIRCLE('',#19420,8.175);
#6440=CIRCLE('',#19421,8.175);
#6441=CIRCLE('',#19422,8.175);
#6442=CIRCLE('',#19423,8.175);
#6443=CIRCLE('',#19424,8.175);
#6444=CIRCLE('',#19425,8.175);
#6445=CIRCLE('',#19426,8.175);
#6446=CIRCLE('',#19427,8.175);
#6447=CIRCLE('',#19428,8.175);
#6448=CIRCLE('',#19429,8.175);
#6449=CIRCLE('',#19430,8.175);
#6450=CIRCLE('',#19431,8.175);
#6451=CIRCLE('',#19432,8.175);
#6452=CIRCLE('',#19433,8.175);
#6453=CIRCLE('',#19434,8.175);
#6454=CIRCLE('',#19435,8.175);
#6455=CIRCLE('',#19436,8.175);
#6456=CIRCLE('',#19437,8.175);
#6457=CIRCLE('',#19438,8.175);
#6458=CIRCLE('',#19439,8.175);
#6459=CIRCLE('',#19440,8.175);
#6460=CIRCLE('',#19441,8.175);
#6461=CIRCLE('',#19442,8.175);
#6462=CIRCLE('',#19443,8.175);
#6463=CIRCLE('',#19444,8.175);
#6464=CIRCLE('',#19445,8.175);
#6465=CIRCLE('',#19446,8.175);
#6466=CIRCLE('',#19447,8.175);
#6467=CIRCLE('',#19448,8.175);
#6468=CIRCLE('',#19449,8.175);
#6469=CIRCLE('',#19450,8.175);
#6470=CIRCLE('',#19451,8.175);
#6471=CIRCLE('',#19452,8.175);
#6472=CIRCLE('',#19453,7.775);
#6473=CIRCLE('',#19454,8.175);
#6474=CIRCLE('',#19455,8.175);
#6475=CIRCLE('',#19456,8.175);
#6476=CIRCLE('',#19457,8.175);
#6477=CIRCLE('',#19458,8.175);
#6478=CIRCLE('',#19459,8.175);
#6479=CIRCLE('',#19460,8.175);
#6480=CIRCLE('',#19461,8.175);
#6481=CIRCLE('',#19462,8.175);
#6482=CIRCLE('',#19463,8.175);
#6483=CIRCLE('',#19464,8.175);
#6484=CIRCLE('',#19465,8.175);
#6485=CIRCLE('',#19466,8.175);
#6486=CIRCLE('',#19467,8.175);
#6487=CIRCLE('',#19468,8.175);
#6488=CIRCLE('',#19469,8.175);
#6489=CIRCLE('',#19470,8.175);
#6490=CIRCLE('',#19471,8.175);
#6491=CIRCLE('',#19472,8.175);
#6492=CIRCLE('',#19473,8.175);
#6493=CIRCLE('',#19474,8.175);
#6494=CIRCLE('',#19475,8.175);
#6495=CIRCLE('',#19476,8.175);
#6496=CIRCLE('',#19477,8.175);
#6497=CIRCLE('',#19478,8.175);
#6498=CIRCLE('',#19479,8.175);
#6499=CIRCLE('',#19480,8.175);
#6500=CIRCLE('',#19481,8.175);
#6501=CIRCLE('',#19482,8.175);
#6502=CIRCLE('',#19483,8.175);
#6503=CIRCLE('',#19484,8.175);
#6504=CIRCLE('',#19485,8.175);
#6505=CIRCLE('',#19486,8.175);
#6506=CIRCLE('',#19487,8.175);
#6507=CIRCLE('',#19488,8.175);
#6508=CIRCLE('',#19489,8.175);
#6509=CIRCLE('',#19490,8.175);
#6510=CIRCLE('',#19491,8.175);
#6511=CIRCLE('',#19493,2.);
#6512=VERTEX_POINT('',#24602);
#6513=VERTEX_POINT('',#24603);
#6514=VERTEX_POINT('',#24605);
#6515=VERTEX_POINT('',#24607);
#6516=VERTEX_POINT('',#24611);
#6517=VERTEX_POINT('',#24612);
#6518=VERTEX_POINT('',#24614);
#6519=VERTEX_POINT('',#24616);
#6520=VERTEX_POINT('',#24620);
#6521=VERTEX_POINT('',#24622);
#6522=VERTEX_POINT('',#24624);
#6523=VERTEX_POINT('',#24626);
#6524=VERTEX_POINT('',#24631);
#6525=VERTEX_POINT('',#24634);
#6526=VERTEX_POINT('',#24636);
#6527=VERTEX_POINT('',#24638);
#6528=VERTEX_POINT('',#24652);
#6529=VERTEX_POINT('',#24653);
#6530=VERTEX_POINT('',#24655);
#6531=VERTEX_POINT('',#24657);
#6532=VERTEX_POINT('',#24661);
#6533=VERTEX_POINT('',#24662);
#6534=VERTEX_POINT('',#24664);
#6535=VERTEX_POINT('',#24666);
#6536=VERTEX_POINT('',#24670);
#6537=VERTEX_POINT('',#24671);
#6538=VERTEX_POINT('',#24673);
#6539=VERTEX_POINT('',#24675);
#6540=VERTEX_POINT('',#24681);
#6541=VERTEX_POINT('',#24683);
#6542=VERTEX_POINT('',#24688);
#6543=VERTEX_POINT('',#24690);
#6544=VERTEX_POINT('',#24702);
#6545=VERTEX_POINT('',#24703);
#6546=VERTEX_POINT('',#24705);
#6547=VERTEX_POINT('',#24707);
#6548=VERTEX_POINT('',#24711);
#6549=VERTEX_POINT('',#24712);
#6550=VERTEX_POINT('',#24715);
#6551=VERTEX_POINT('',#24717);
#6552=VERTEX_POINT('',#24719);
#6553=VERTEX_POINT('',#24721);
#6554=VERTEX_POINT('',#24725);
#6555=VERTEX_POINT('',#24727);
#6556=VERTEX_POINT('',#24729);
#6557=VERTEX_POINT('',#24731);
#6558=VERTEX_POINT('',#24733);
#6559=VERTEX_POINT('',#24735);
#6560=VERTEX_POINT('',#24752);
#6561=VERTEX_POINT('',#24753);
#6562=VERTEX_POINT('',#24755);
#6563=VERTEX_POINT('',#24757);
#6564=VERTEX_POINT('',#24761);
#6565=VERTEX_POINT('',#24762);
#6566=VERTEX_POINT('',#24765);
#6567=VERTEX_POINT('',#24767);
#6568=VERTEX_POINT('',#24769);
#6569=VERTEX_POINT('',#24771);
#6570=VERTEX_POINT('',#24775);
#6571=VERTEX_POINT('',#24777);
#6572=VERTEX_POINT('',#24779);
#6573=VERTEX_POINT('',#24781);
#6574=VERTEX_POINT('',#24783);
#6575=VERTEX_POINT('',#24785);
#6576=VERTEX_POINT('',#24803);
#6577=VERTEX_POINT('',#24804);
#6578=VERTEX_POINT('',#24806);
#6579=VERTEX_POINT('',#24808);
#6580=VERTEX_POINT('',#24812);
#6581=VERTEX_POINT('',#24813);
#6582=VERTEX_POINT('',#24817);
#6583=VERTEX_POINT('',#24820);
#6584=VERTEX_POINT('',#24829);
#6585=VERTEX_POINT('',#24830);
#6586=VERTEX_POINT('',#24832);
#6587=VERTEX_POINT('',#24834);
#6588=VERTEX_POINT('',#24838);
#6589=VERTEX_POINT('',#24839);
#6590=VERTEX_POINT('',#24841);
#6591=VERTEX_POINT('',#24843);
#6592=VERTEX_POINT('',#24855);
#6593=VERTEX_POINT('',#24856);
#6594=VERTEX_POINT('',#24858);
#6595=VERTEX_POINT('',#24860);
#6596=VERTEX_POINT('',#24864);
#6597=VERTEX_POINT('',#24865);
#6598=VERTEX_POINT('',#24867);
#6599=VERTEX_POINT('',#24869);
#6600=VERTEX_POINT('',#24871);
#6601=VERTEX_POINT('',#24873);
#6602=VERTEX_POINT('',#24878);
#6603=VERTEX_POINT('',#24879);
#6604=VERTEX_POINT('',#24884);
#6605=VERTEX_POINT('',#24886);
#6606=VERTEX_POINT('',#24888);
#6607=VERTEX_POINT('',#24890);
#6608=VERTEX_POINT('',#24905);
#6609=VERTEX_POINT('',#24906);
#6610=VERTEX_POINT('',#24910);
#6611=VERTEX_POINT('',#24947);
#6612=VERTEX_POINT('',#24949);
#6613=VERTEX_POINT('',#24953);
#6614=VERTEX_POINT('',#24954);
#6615=VERTEX_POINT('',#24957);
#6616=VERTEX_POINT('',#24961);
#6617=VERTEX_POINT('',#24965);
#6618=VERTEX_POINT('',#24973);
#6619=VERTEX_POINT('',#24974);
#6620=VERTEX_POINT('',#24976);
#6621=VERTEX_POINT('',#24984);
#6622=VERTEX_POINT('',#24994);
#6623=VERTEX_POINT('',#24995);
#6624=VERTEX_POINT('',#25024);
#6625=VERTEX_POINT('',#25025);
#6626=VERTEX_POINT('',#25054);
#6627=VERTEX_POINT('',#25055);
#6628=VERTEX_POINT('',#25084);
#6629=VERTEX_POINT('',#25085);
#6630=VERTEX_POINT('',#25114);
#6631=VERTEX_POINT('',#25115);
#6632=VERTEX_POINT('',#25144);
#6633=VERTEX_POINT('',#25145);
#6634=VERTEX_POINT('',#25174);
#6635=VERTEX_POINT('',#25175);
#6636=VERTEX_POINT('',#25204);
#6637=VERTEX_POINT('',#25205);
#6638=VERTEX_POINT('',#25234);
#6639=VERTEX_POINT('',#25235);
#6640=VERTEX_POINT('',#25264);
#6641=VERTEX_POINT('',#25265);
#6642=VERTEX_POINT('',#25294);
#6643=VERTEX_POINT('',#25295);
#6644=VERTEX_POINT('',#25324);
#6645=VERTEX_POINT('',#25325);
#6646=VERTEX_POINT('',#25354);
#6647=VERTEX_POINT('',#25355);
#6648=VERTEX_POINT('',#25384);
#6649=VERTEX_POINT('',#25385);
#6650=VERTEX_POINT('',#25414);
#6651=VERTEX_POINT('',#25415);
#6652=VERTEX_POINT('',#25444);
#6653=VERTEX_POINT('',#25445);
#6654=VERTEX_POINT('',#25474);
#6655=VERTEX_POINT('',#25475);
#6656=VERTEX_POINT('',#25504);
#6657=VERTEX_POINT('',#25505);
#6658=VERTEX_POINT('',#25534);
#6659=VERTEX_POINT('',#25535);
#6660=VERTEX_POINT('',#25564);
#6661=VERTEX_POINT('',#25565);
#6662=VERTEX_POINT('',#25594);
#6663=VERTEX_POINT('',#25595);
#6664=VERTEX_POINT('',#25624);
#6665=VERTEX_POINT('',#25625);
#6666=VERTEX_POINT('',#25654);
#6667=VERTEX_POINT('',#25655);
#6668=VERTEX_POINT('',#25684);
#6669=VERTEX_POINT('',#25685);
#6670=VERTEX_POINT('',#25687);
#6671=VERTEX_POINT('',#25693);
#6672=VERTEX_POINT('',#25701);
#6673=VERTEX_POINT('',#25702);
#6674=VERTEX_POINT('',#25704);
#6675=VERTEX_POINT('',#25743);
#6676=VERTEX_POINT('',#25744);
#6677=VERTEX_POINT('',#25746);
#6678=VERTEX_POINT('',#25824);
#6679=VERTEX_POINT('',#25825);
#6680=VERTEX_POINT('',#25900);
#6681=VERTEX_POINT('',#25901);
#6682=VERTEX_POINT('',#25976);
#6683=VERTEX_POINT('',#25977);
#6684=VERTEX_POINT('',#26052);
#6685=VERTEX_POINT('',#26053);
#6686=VERTEX_POINT('',#26128);
#6687=VERTEX_POINT('',#26129);
#6688=VERTEX_POINT('',#26206);
#6689=VERTEX_POINT('',#26207);
#6690=VERTEX_POINT('',#26284);
#6691=VERTEX_POINT('',#26285);
#6692=VERTEX_POINT('',#26360);
#6693=VERTEX_POINT('',#26361);
#6694=VERTEX_POINT('',#26436);
#6695=VERTEX_POINT('',#26437);
#6696=VERTEX_POINT('',#26512);
#6697=VERTEX_POINT('',#26513);
#6698=VERTEX_POINT('',#26588);
#6699=VERTEX_POINT('',#26589);
#6700=VERTEX_POINT('',#26668);
#6701=VERTEX_POINT('',#26669);
#6702=VERTEX_POINT('',#26744);
#6703=VERTEX_POINT('',#26745);
#6704=VERTEX_POINT('',#26820);
#6705=VERTEX_POINT('',#26821);
#6706=VERTEX_POINT('',#26896);
#6707=VERTEX_POINT('',#26897);
#6708=VERTEX_POINT('',#26972);
#6709=VERTEX_POINT('',#26973);
#6710=VERTEX_POINT('',#27048);
#6711=VERTEX_POINT('',#27049);
#6712=VERTEX_POINT('',#27128);
#6713=VERTEX_POINT('',#27129);
#6714=VERTEX_POINT('',#27204);
#6715=VERTEX_POINT('',#27205);
#6716=VERTEX_POINT('',#27280);
#6717=VERTEX_POINT('',#27281);
#6718=VERTEX_POINT('',#27356);
#6719=VERTEX_POINT('',#27357);
#6720=VERTEX_POINT('',#27432);
#6721=VERTEX_POINT('',#27433);
#6722=VERTEX_POINT('',#27508);
#6723=VERTEX_POINT('',#27509);
#6724=VERTEX_POINT('',#27511);
#6725=VERTEX_POINT('',#27520);
#6726=VERTEX_POINT('',#27539);
#6727=VERTEX_POINT('',#27543);
#6728=VERTEX_POINT('',#27545);
#6729=VERTEX_POINT('',#27547);
#6730=VERTEX_POINT('',#27549);
#6731=VERTEX_POINT('',#27584);
#6732=VERTEX_POINT('',#27586);
#6733=VERTEX_POINT('',#27589);
#6734=VERTEX_POINT('',#27591);
#6735=VERTEX_POINT('',#27628);
#6736=VERTEX_POINT('',#27630);
#6737=VERTEX_POINT('',#27634);
#6738=VERTEX_POINT('',#27636);
#6739=VERTEX_POINT('',#27638);
#6740=VERTEX_POINT('',#27640);
#6741=VERTEX_POINT('',#27813);
#6742=VERTEX_POINT('',#27816);
#6743=VERTEX_POINT('',#27818);
#6744=VERTEX_POINT('',#27993);
#6745=VERTEX_POINT('',#27995);
#6746=VERTEX_POINT('',#27999);
#6747=VERTEX_POINT('',#28003);
#6748=VERTEX_POINT('',#28005);
#6749=VERTEX_POINT('',#29888);
#6750=VERTEX_POINT('',#29890);
#6751=VERTEX_POINT('',#29894);
#6752=VERTEX_POINT('',#29896);
#6753=VERTEX_POINT('',#29904);
#6754=VERTEX_POINT('',#29906);
#6755=VERTEX_POINT('',#29910);
#6756=VERTEX_POINT('',#29912);
#6757=VERTEX_POINT('',#29919);
#6758=VERTEX_POINT('',#29920);
#6759=VERTEX_POINT('',#29923);
#6760=VERTEX_POINT('',#29927);
#6761=VERTEX_POINT('',#29929);
#6762=VERTEX_POINT('',#29933);
#6763=VERTEX_POINT('',#29942);
#6764=VERTEX_POINT('',#29944);
#6765=VERTEX_POINT('',#29948);
#6766=VERTEX_POINT('',#29952);
#6767=VERTEX_POINT('',#29956);
#6768=VERTEX_POINT('',#29958);
#6769=VERTEX_POINT('',#29962);
#6770=VERTEX_POINT('',#29966);
#6771=VERTEX_POINT('',#29967);
#6772=VERTEX_POINT('',#29969);
#6773=VERTEX_POINT('',#29972);
#6774=VERTEX_POINT('',#29980);
#6775=VERTEX_POINT('',#29982);
#6776=VERTEX_POINT('',#29986);
#6777=VERTEX_POINT('',#29987);
#6778=VERTEX_POINT('',#29989);
#6779=VERTEX_POINT('',#29993);
#6780=VERTEX_POINT('',#29995);
#6781=VERTEX_POINT('',#29999);
#6782=VERTEX_POINT('',#30001);
#6783=VERTEX_POINT('',#30012);
#6784=VERTEX_POINT('',#30014);
#6785=VERTEX_POINT('',#30027);
#6786=VERTEX_POINT('',#30028);
#6787=VERTEX_POINT('',#30159);
#6788=VERTEX_POINT('',#30227);
#6789=VERTEX_POINT('',#30295);
#6790=VERTEX_POINT('',#30297);
#6791=VERTEX_POINT('',#30302);
#6792=VERTEX_POINT('',#30304);
#6793=VERTEX_POINT('',#30308);
#6794=VERTEX_POINT('',#30309);
#6795=VERTEX_POINT('',#30437);
#6796=VERTEX_POINT('',#30444);
#6797=VERTEX_POINT('',#30447);
#6798=VERTEX_POINT('',#30449);
#6799=VERTEX_POINT('',#30594);
#6800=VERTEX_POINT('',#30610);
#6801=VERTEX_POINT('',#30627);
#6802=VERTEX_POINT('',#30629);
#6803=VERTEX_POINT('',#30640);
#6804=VERTEX_POINT('',#30643);
#6805=VERTEX_POINT('',#30661);
#6806=VERTEX_POINT('',#30741);
#6807=VERTEX_POINT('',#30758);
#6808=VERTEX_POINT('',#30766);
#6809=VERTEX_POINT('',#30768);
#6810=VERTEX_POINT('',#30783);
#6811=VERTEX_POINT('',#31028);
#6812=VERTEX_POINT('',#31043);
#6813=VERTEX_POINT('',#31045);
#6814=VERTEX_POINT('',#31053);
#6815=VERTEX_POINT('',#31237);
#6816=VERTEX_POINT('',#31239);
#6817=VERTEX_POINT('',#31243);
#6818=VERTEX_POINT('',#31245);
#6819=VERTEX_POINT('',#31249);
#6820=VERTEX_POINT('',#32002);
#6821=VERTEX_POINT('',#32003);
#6822=VERTEX_POINT('',#32005);
#6823=VERTEX_POINT('',#32007);
#6824=VERTEX_POINT('',#32011);
#6825=VERTEX_POINT('',#32013);
#6826=VERTEX_POINT('',#32021);
#6827=VERTEX_POINT('',#32025);
#6828=VERTEX_POINT('',#32029);
#6829=VERTEX_POINT('',#32037);
#6830=VERTEX_POINT('',#32038);
#6831=VERTEX_POINT('',#32040);
#6832=VERTEX_POINT('',#32045);
#6833=VERTEX_POINT('',#32066);
#6834=VERTEX_POINT('',#32068);
#6835=VERTEX_POINT('',#32070);
#6836=VERTEX_POINT('',#32132);
#6837=VERTEX_POINT('',#32133);
#6838=VERTEX_POINT('',#32135);
#6839=VERTEX_POINT('',#32137);
#6840=VERTEX_POINT('',#32139);
#6841=VERTEX_POINT('',#32158);
#6842=VERTEX_POINT('',#32274);
#6843=VERTEX_POINT('',#32276);
#6844=VERTEX_POINT('',#32280);
#6845=VERTEX_POINT('',#32281);
#6846=VERTEX_POINT('',#32283);
#6847=VERTEX_POINT('',#32381);
#6848=VERTEX_POINT('',#32383);
#6849=VERTEX_POINT('',#32481);
#6850=VERTEX_POINT('',#32489);
#6851=VERTEX_POINT('',#32493);
#6852=VERTEX_POINT('',#32496);
#6853=VERTEX_POINT('',#32498);
#6854=VERTEX_POINT('',#32534);
#6855=VERTEX_POINT('',#32536);
#6856=VERTEX_POINT('',#32538);
#6857=VERTEX_POINT('',#32541);
#6858=VERTEX_POINT('',#32546);
#6859=VERTEX_POINT('',#32548);
#6860=VERTEX_POINT('',#32609);
#6861=VERTEX_POINT('',#32614);
#6862=VERTEX_POINT('',#32616);
#6863=VERTEX_POINT('',#32976);
#6864=VERTEX_POINT('',#32977);
#6865=VERTEX_POINT('',#32979);
#6866=VERTEX_POINT('',#32981);
#6867=VERTEX_POINT('',#32985);
#6868=VERTEX_POINT('',#32987);
#6869=VERTEX_POINT('',#32995);
#6870=VERTEX_POINT('',#32999);
#6871=VERTEX_POINT('',#33003);
#6872=VERTEX_POINT('',#33011);
#6873=VERTEX_POINT('',#33012);
#6874=VERTEX_POINT('',#33015);
#6875=VERTEX_POINT('',#33019);
#6876=VERTEX_POINT('',#33021);
#6877=VERTEX_POINT('',#33025);
#6878=VERTEX_POINT('',#33026);
#6879=VERTEX_POINT('',#33031);
#6880=VERTEX_POINT('',#33033);
#6881=VERTEX_POINT('',#33037);
#6882=VERTEX_POINT('',#33041);
#6883=VERTEX_POINT('',#33043);
#6884=VERTEX_POINT('',#33047);
#6885=VERTEX_POINT('',#33056);
#6886=VERTEX_POINT('',#33057);
#6887=VERTEX_POINT('',#33059);
#6888=VERTEX_POINT('',#33061);
#6889=VERTEX_POINT('',#33065);
#6890=VERTEX_POINT('',#33066);
#6891=VERTEX_POINT('',#33068);
#6892=VERTEX_POINT('',#33070);
#6893=VERTEX_POINT('',#33074);
#6894=VERTEX_POINT('',#33076);
#6895=VERTEX_POINT('',#33078);
#6896=VERTEX_POINT('',#33082);
#6897=VERTEX_POINT('',#33083);
#6898=VERTEX_POINT('',#33085);
#6899=VERTEX_POINT('',#33087);
#6900=VERTEX_POINT('',#33091);
#6901=VERTEX_POINT('',#33092);
#6902=VERTEX_POINT('',#33094);
#6903=VERTEX_POINT('',#33096);
#6904=VERTEX_POINT('',#33100);
#6905=VERTEX_POINT('',#33102);
#6906=VERTEX_POINT('',#33104);
#6907=VERTEX_POINT('',#33108);
#6908=VERTEX_POINT('',#33109);
#6909=VERTEX_POINT('',#33111);
#6910=VERTEX_POINT('',#33113);
#6911=VERTEX_POINT('',#33117);
#6912=VERTEX_POINT('',#33119);
#6913=VERTEX_POINT('',#33121);
#6914=VERTEX_POINT('',#33125);
#6915=VERTEX_POINT('',#33126);
#6916=VERTEX_POINT('',#33128);
#6917=VERTEX_POINT('',#33130);
#6918=VERTEX_POINT('',#33134);
#6919=VERTEX_POINT('',#33135);
#6920=VERTEX_POINT('',#33137);
#6921=VERTEX_POINT('',#33142);
#6922=VERTEX_POINT('',#33146);
#6923=VERTEX_POINT('',#33150);
#6924=VERTEX_POINT('',#33152);
#6925=VERTEX_POINT('',#33156);
#6926=VERTEX_POINT('',#33158);
#6927=VERTEX_POINT('',#33162);
#6928=VERTEX_POINT('',#33164);
#6929=VERTEX_POINT('',#33168);
#6930=VERTEX_POINT('',#33169);
#6931=VERTEX_POINT('',#33171);
#6932=VERTEX_POINT('',#33173);
#6933=VERTEX_POINT('',#33177);
#6934=VERTEX_POINT('',#33179);
#6935=VERTEX_POINT('',#33186);
#6936=VERTEX_POINT('',#33188);
#6937=VERTEX_POINT('',#33192);
#6938=VERTEX_POINT('',#33193);
#6939=VERTEX_POINT('',#33195);
#6940=VERTEX_POINT('',#33197);
#6941=VERTEX_POINT('',#33201);
#6942=VERTEX_POINT('',#33202);
#6943=VERTEX_POINT('',#33207);
#6944=VERTEX_POINT('',#33208);
#6945=VERTEX_POINT('',#33213);
#6946=VERTEX_POINT('',#33222);
#6947=VERTEX_POINT('',#33223);
#6948=VERTEX_POINT('',#33226);
#6949=VERTEX_POINT('',#33238);
#6950=VERTEX_POINT('',#33243);
#6951=VERTEX_POINT('',#33244);
#6952=VERTEX_POINT('',#33249);
#6953=VERTEX_POINT('',#33251);
#6954=VERTEX_POINT('',#33253);
#6955=VERTEX_POINT('',#33266);
#6956=VERTEX_POINT('',#33268);
#6957=VERTEX_POINT('',#33280);
#6958=VERTEX_POINT('',#33282);
#6959=VERTEX_POINT('',#33286);
#6960=VERTEX_POINT('',#33290);
#6961=VERTEX_POINT('',#33361);
#6962=VERTEX_POINT('',#33363);
#6963=VERTEX_POINT('',#33367);
#6964=VERTEX_POINT('',#33368);
#6965=VERTEX_POINT('',#33371);
#6966=VERTEX_POINT('',#33375);
#6967=VERTEX_POINT('',#33376);
#6968=VERTEX_POINT('',#33379);
#6969=VERTEX_POINT('',#33383);
#6970=VERTEX_POINT('',#33385);
#6971=VERTEX_POINT('',#33389);
#6972=VERTEX_POINT('',#33390);
#6973=VERTEX_POINT('',#33392);
#6974=VERTEX_POINT('',#33396);
#6975=VERTEX_POINT('',#33402);
#6976=VERTEX_POINT('',#33403);
#6977=VERTEX_POINT('',#33406);
#6978=VERTEX_POINT('',#33410);
#6979=VERTEX_POINT('',#33411);
#6980=VERTEX_POINT('',#33414);
#6981=VERTEX_POINT('',#33418);
#6982=VERTEX_POINT('',#33420);
#6983=VERTEX_POINT('',#33424);
#6984=VERTEX_POINT('',#33426);
#6985=VERTEX_POINT('',#33430);
#6986=VERTEX_POINT('',#33431);
#6987=VERTEX_POINT('',#33433);
#6988=VERTEX_POINT('',#33437);
#6989=VERTEX_POINT('',#33443);
#6990=VERTEX_POINT('',#33445);
#6991=VERTEX_POINT('',#33447);
#6992=VERTEX_POINT('',#33477);
#6993=VERTEX_POINT('',#33491);
#6994=VERTEX_POINT('',#33492);
#6995=VERTEX_POINT('',#33494);
#6996=VERTEX_POINT('',#33496);
#6997=VERTEX_POINT('',#33500);
#6998=VERTEX_POINT('',#33501);
#6999=VERTEX_POINT('',#33503);
#7000=VERTEX_POINT('',#33505);
#7001=VERTEX_POINT('',#33509);
#7002=VERTEX_POINT('',#33511);
#7003=VERTEX_POINT('',#33513);
#7004=VERTEX_POINT('',#33515);
#7005=VERTEX_POINT('',#33518);
#7006=VERTEX_POINT('',#33520);
#7007=VERTEX_POINT('',#33522);
#7008=VERTEX_POINT('',#33524);
#7009=VERTEX_POINT('',#33526);
#7010=VERTEX_POINT('',#33528);
#7011=VERTEX_POINT('',#33530);
#7012=VERTEX_POINT('',#33532);
#7013=VERTEX_POINT('',#33536);
#7014=VERTEX_POINT('',#33538);
#7015=VERTEX_POINT('',#33542);
#7016=VERTEX_POINT('',#33544);
#7017=VERTEX_POINT('',#33546);
#7018=VERTEX_POINT('',#33548);
#7019=VERTEX_POINT('',#33550);
#7020=VERTEX_POINT('',#33553);
#7021=VERTEX_POINT('',#33555);
#7022=VERTEX_POINT('',#33557);
#7023=VERTEX_POINT('',#33559);
#7024=VERTEX_POINT('',#33561);
#7025=VERTEX_POINT('',#33563);
#7026=VERTEX_POINT('',#33566);
#7027=VERTEX_POINT('',#33568);
#7028=VERTEX_POINT('',#33570);
#7029=VERTEX_POINT('',#33574);
#7030=VERTEX_POINT('',#33575);
#7031=VERTEX_POINT('',#33577);
#7032=VERTEX_POINT('',#33579);
#7033=VERTEX_POINT('',#33583);
#7034=VERTEX_POINT('',#33584);
#7035=VERTEX_POINT('',#33586);
#7036=VERTEX_POINT('',#33588);
#7037=VERTEX_POINT('',#33590);
#7038=VERTEX_POINT('',#33592);
#7039=VERTEX_POINT('',#33597);
#7040=VERTEX_POINT('',#33598);
#7041=VERTEX_POINT('',#33600);
#7042=VERTEX_POINT('',#33602);
#7043=VERTEX_POINT('',#33604);
#7044=VERTEX_POINT('',#33606);
#7045=VERTEX_POINT('',#33608);
#7046=VERTEX_POINT('',#33612);
#7047=VERTEX_POINT('',#33613);
#7048=VERTEX_POINT('',#33615);
#7049=VERTEX_POINT('',#33617);
#7050=VERTEX_POINT('',#33619);
#7051=VERTEX_POINT('',#33621);
#7052=VERTEX_POINT('',#33623);
#7053=VERTEX_POINT('',#33625);
#7054=VERTEX_POINT('',#33627);
#7055=VERTEX_POINT('',#33631);
#7056=VERTEX_POINT('',#33632);
#7057=VERTEX_POINT('',#33634);
#7058=VERTEX_POINT('',#33636);
#7059=VERTEX_POINT('',#33649);
#7060=VERTEX_POINT('',#33650);
#7061=VERTEX_POINT('',#33661);
#7062=VERTEX_POINT('',#33662);
#7063=VERTEX_POINT('',#33693);
#7064=VERTEX_POINT('',#33695);
#7065=VERTEX_POINT('',#33697);
#7066=VERTEX_POINT('',#33699);
#7067=VERTEX_POINT('',#33703);
#7068=VERTEX_POINT('',#33707);
#7069=VERTEX_POINT('',#33709);
#7070=VERTEX_POINT('',#33713);
#7071=VERTEX_POINT('',#33719);
#7072=VERTEX_POINT('',#33720);
#7073=VERTEX_POINT('',#33725);
#7074=VERTEX_POINT('',#33726);
#7075=VERTEX_POINT('',#33798);
#7076=VERTEX_POINT('',#33800);
#7077=VERTEX_POINT('',#33802);
#7078=VERTEX_POINT('',#33806);
#7079=VERTEX_POINT('',#33807);
#7080=VERTEX_POINT('',#33810);
#7081=VERTEX_POINT('',#33818);
#7082=VERTEX_POINT('',#33820);
#7083=VERTEX_POINT('',#33824);
#7084=VERTEX_POINT('',#33825);
#7085=VERTEX_POINT('',#33827);
#7086=VERTEX_POINT('',#33829);
#7087=VERTEX_POINT('',#33834);
#7088=VERTEX_POINT('',#33836);
#7089=VERTEX_POINT('',#33840);
#7090=VERTEX_POINT('',#33842);
#7091=VERTEX_POINT('',#33846);
#7092=VERTEX_POINT('',#33848);
#7093=VERTEX_POINT('',#33852);
#7094=VERTEX_POINT('',#33854);
#7095=VERTEX_POINT('',#33858);
#7096=VERTEX_POINT('',#33860);
#7097=VERTEX_POINT('',#33864);
#7098=VERTEX_POINT('',#33865);
#7099=VERTEX_POINT('',#33867);
#7100=VERTEX_POINT('',#33869);
#7101=VERTEX_POINT('',#33873);
#7102=VERTEX_POINT('',#33875);
#7103=VERTEX_POINT('',#33882);
#7104=VERTEX_POINT('',#33883);
#7105=VERTEX_POINT('',#33885);
#7106=VERTEX_POINT('',#33887);
#7107=VERTEX_POINT('',#33889);
#7108=VERTEX_POINT('',#33896);
#7109=VERTEX_POINT('',#33897);
#7110=VERTEX_POINT('',#33900);
#7111=VERTEX_POINT('',#33904);
#7112=VERTEX_POINT('',#33908);
#7113=VERTEX_POINT('',#33912);
#7114=VERTEX_POINT('',#33914);
#7115=VERTEX_POINT('',#33926);
#7116=VERTEX_POINT('',#33928);
#7117=VERTEX_POINT('',#33932);
#7118=VERTEX_POINT('',#33933);
#7119=VERTEX_POINT('',#33937);
#7120=VERTEX_POINT('',#33939);
#7121=VERTEX_POINT('',#33943);
#7122=VERTEX_POINT('',#33944);
#7123=VERTEX_POINT('',#33947);
#7124=VERTEX_POINT('',#33951);
#7125=VERTEX_POINT('',#33952);
#7126=VERTEX_POINT('',#33955);
#7127=VERTEX_POINT('',#33957);
#7128=VERTEX_POINT('',#33963);
#7129=VERTEX_POINT('',#33964);
#7130=VERTEX_POINT('',#33969);
#7131=VERTEX_POINT('',#33970);
#7132=VERTEX_POINT('',#33973);
#7133=VERTEX_POINT('',#33975);
#7134=VERTEX_POINT('',#33981);
#7135=VERTEX_POINT('',#33982);
#7136=VERTEX_POINT('',#33987);
#7137=VERTEX_POINT('',#33988);
#7138=VERTEX_POINT('',#33991);
#7139=VERTEX_POINT('',#33993);
#7140=VERTEX_POINT('',#33999);
#7141=VERTEX_POINT('',#34000);
#7142=VERTEX_POINT('',#34005);
#7143=VERTEX_POINT('',#34006);
#7144=VERTEX_POINT('',#34009);
#7145=VERTEX_POINT('',#34011);
#7146=VERTEX_POINT('',#34017);
#7147=VERTEX_POINT('',#34018);
#7148=VERTEX_POINT('',#34023);
#7149=VERTEX_POINT('',#34024);
#7150=VERTEX_POINT('',#34027);
#7151=VERTEX_POINT('',#34029);
#7152=VERTEX_POINT('',#34035);
#7153=VERTEX_POINT('',#34036);
#7154=VERTEX_POINT('',#34041);
#7155=VERTEX_POINT('',#34042);
#7156=VERTEX_POINT('',#34045);
#7157=VERTEX_POINT('',#34047);
#7158=VERTEX_POINT('',#34053);
#7159=VERTEX_POINT('',#34054);
#7160=VERTEX_POINT('',#34059);
#7161=VERTEX_POINT('',#34060);
#7162=VERTEX_POINT('',#34063);
#7163=VERTEX_POINT('',#34065);
#7164=VERTEX_POINT('',#34071);
#7165=VERTEX_POINT('',#34072);
#7166=VERTEX_POINT('',#34077);
#7167=VERTEX_POINT('',#34078);
#7168=VERTEX_POINT('',#34081);
#7169=VERTEX_POINT('',#34083);
#7170=VERTEX_POINT('',#34089);
#7171=VERTEX_POINT('',#34090);
#7172=VERTEX_POINT('',#34095);
#7173=VERTEX_POINT('',#34096);
#7174=VERTEX_POINT('',#34099);
#7175=VERTEX_POINT('',#34101);
#7176=VERTEX_POINT('',#34107);
#7177=VERTEX_POINT('',#34108);
#7178=VERTEX_POINT('',#34113);
#7179=VERTEX_POINT('',#34114);
#7180=VERTEX_POINT('',#34117);
#7181=VERTEX_POINT('',#34119);
#7182=VERTEX_POINT('',#34125);
#7183=VERTEX_POINT('',#34126);
#7184=VERTEX_POINT('',#34131);
#7185=VERTEX_POINT('',#34132);
#7186=VERTEX_POINT('',#34135);
#7187=VERTEX_POINT('',#34137);
#7188=VERTEX_POINT('',#34143);
#7189=VERTEX_POINT('',#34144);
#7190=VERTEX_POINT('',#34149);
#7191=VERTEX_POINT('',#34150);
#7192=VERTEX_POINT('',#34153);
#7193=VERTEX_POINT('',#34155);
#7194=VERTEX_POINT('',#34161);
#7195=VERTEX_POINT('',#34162);
#7196=VERTEX_POINT('',#34167);
#7197=VERTEX_POINT('',#34168);
#7198=VERTEX_POINT('',#34171);
#7199=VERTEX_POINT('',#34173);
#7200=VERTEX_POINT('',#34179);
#7201=VERTEX_POINT('',#34180);
#7202=VERTEX_POINT('',#34185);
#7203=VERTEX_POINT('',#34186);
#7204=VERTEX_POINT('',#34189);
#7205=VERTEX_POINT('',#34191);
#7206=VERTEX_POINT('',#34197);
#7207=VERTEX_POINT('',#34198);
#7208=VERTEX_POINT('',#34203);
#7209=VERTEX_POINT('',#34204);
#7210=VERTEX_POINT('',#34207);
#7211=VERTEX_POINT('',#34209);
#7212=VERTEX_POINT('',#34215);
#7213=VERTEX_POINT('',#34216);
#7214=VERTEX_POINT('',#34220);
#7215=VERTEX_POINT('',#34222);
#7216=VERTEX_POINT('',#34226);
#7217=VERTEX_POINT('',#34230);
#7218=VERTEX_POINT('',#34232);
#7219=VERTEX_POINT('',#34236);
#7220=VERTEX_POINT('',#34240);
#7221=VERTEX_POINT('',#34242);
#7222=VERTEX_POINT('',#34246);
#7223=VERTEX_POINT('',#34250);
#7224=VERTEX_POINT('',#34252);
#7225=VERTEX_POINT('',#34256);
#7226=VERTEX_POINT('',#34260);
#7227=VERTEX_POINT('',#34262);
#7228=VERTEX_POINT('',#34266);
#7229=VERTEX_POINT('',#34270);
#7230=VERTEX_POINT('',#34272);
#7231=VERTEX_POINT('',#34276);
#7232=VERTEX_POINT('',#34280);
#7233=VERTEX_POINT('',#34282);
#7234=VERTEX_POINT('',#34286);
#7235=VERTEX_POINT('',#34290);
#7236=VERTEX_POINT('',#34292);
#7237=VERTEX_POINT('',#34296);
#7238=VERTEX_POINT('',#34300);
#7239=VERTEX_POINT('',#34302);
#7240=VERTEX_POINT('',#34306);
#7241=VERTEX_POINT('',#34310);
#7242=VERTEX_POINT('',#34312);
#7243=VERTEX_POINT('',#34316);
#7244=VERTEX_POINT('',#34320);
#7245=VERTEX_POINT('',#34322);
#7246=VERTEX_POINT('',#34326);
#7247=VERTEX_POINT('',#34330);
#7248=VERTEX_POINT('',#34332);
#7249=VERTEX_POINT('',#34336);
#7250=VERTEX_POINT('',#34340);
#7251=VERTEX_POINT('',#34342);
#7252=VERTEX_POINT('',#34346);
#7253=VERTEX_POINT('',#34350);
#7254=VERTEX_POINT('',#34352);
#7255=VERTEX_POINT('',#34356);
#7256=VERTEX_POINT('',#34360);
#7257=VERTEX_POINT('',#34362);
#7258=VERTEX_POINT('',#34366);
#7259=VERTEX_POINT('',#34370);
#7260=VERTEX_POINT('',#34372);
#7261=VERTEX_POINT('',#34376);
#7262=VERTEX_POINT('',#34380);
#7263=VERTEX_POINT('',#34382);
#7264=VERTEX_POINT('',#34386);
#7265=VERTEX_POINT('',#34390);
#7266=VERTEX_POINT('',#34392);
#7267=VERTEX_POINT('',#34396);
#7268=VERTEX_POINT('',#34400);
#7269=VERTEX_POINT('',#34402);
#7270=VERTEX_POINT('',#34406);
#7271=VERTEX_POINT('',#34410);
#7272=VERTEX_POINT('',#34412);
#7273=VERTEX_POINT('',#34416);
#7274=VERTEX_POINT('',#34420);
#7275=VERTEX_POINT('',#34422);
#7276=VERTEX_POINT('',#34426);
#7277=VERTEX_POINT('',#34430);
#7278=VERTEX_POINT('',#34432);
#7279=VERTEX_POINT('',#34436);
#7280=VERTEX_POINT('',#34440);
#7281=VERTEX_POINT('',#34442);
#7282=VERTEX_POINT('',#34446);
#7283=VERTEX_POINT('',#34450);
#7284=VERTEX_POINT('',#34452);
#7285=VERTEX_POINT('',#34456);
#7286=VERTEX_POINT('',#34460);
#7287=VERTEX_POINT('',#34462);
#7288=VERTEX_POINT('',#34466);
#7289=VERTEX_POINT('',#34470);
#7290=VERTEX_POINT('',#34472);
#7291=VERTEX_POINT('',#34476);
#7292=VERTEX_POINT('',#34480);
#7293=VERTEX_POINT('',#34482);
#7294=VERTEX_POINT('',#34486);
#7295=VERTEX_POINT('',#34490);
#7296=VERTEX_POINT('',#34492);
#7297=VERTEX_POINT('',#34496);
#7298=VERTEX_POINT('',#34500);
#7299=VERTEX_POINT('',#34502);
#7300=VERTEX_POINT('',#34506);
#7301=VERTEX_POINT('',#34510);
#7302=VERTEX_POINT('',#34512);
#7303=VERTEX_POINT('',#34516);
#7304=VERTEX_POINT('',#34520);
#7305=VERTEX_POINT('',#34522);
#7306=VERTEX_POINT('',#34526);
#7307=VERTEX_POINT('',#34530);
#7308=VERTEX_POINT('',#34532);
#7309=VERTEX_POINT('',#34536);
#7310=VERTEX_POINT('',#34540);
#7311=VERTEX_POINT('',#34542);
#7312=VERTEX_POINT('',#34546);
#7313=VERTEX_POINT('',#34550);
#7314=VERTEX_POINT('',#34552);
#7315=VERTEX_POINT('',#34556);
#7316=VERTEX_POINT('',#34560);
#7317=VERTEX_POINT('',#34562);
#7318=VERTEX_POINT('',#34566);
#7319=VERTEX_POINT('',#34570);
#7320=VERTEX_POINT('',#34572);
#7321=VERTEX_POINT('',#34576);
#7322=VERTEX_POINT('',#34580);
#7323=VERTEX_POINT('',#34582);
#7324=VERTEX_POINT('',#34586);
#7325=VERTEX_POINT('',#34590);
#7326=VERTEX_POINT('',#34592);
#7327=VERTEX_POINT('',#34596);
#7328=VERTEX_POINT('',#34600);
#7329=VERTEX_POINT('',#34602);
#7330=VERTEX_POINT('',#34606);
#7331=VERTEX_POINT('',#34609);
#7332=VERTEX_POINT('',#34613);
#7333=VERTEX_POINT('',#34617);
#7334=VERTEX_POINT('',#34619);
#7335=VERTEX_POINT('',#34623);
#7336=VERTEX_POINT('',#34627);
#7337=VERTEX_POINT('',#34629);
#7338=VERTEX_POINT('',#34633);
#7339=VERTEX_POINT('',#34637);
#7340=VERTEX_POINT('',#34639);
#7341=VERTEX_POINT('',#34643);
#7342=VERTEX_POINT('',#34647);
#7343=VERTEX_POINT('',#34649);
#7344=VERTEX_POINT('',#34653);
#7345=VERTEX_POINT('',#34657);
#7346=VERTEX_POINT('',#34659);
#7347=VERTEX_POINT('',#34663);
#7348=VERTEX_POINT('',#34667);
#7349=VERTEX_POINT('',#34669);
#7350=VERTEX_POINT('',#34673);
#7351=VERTEX_POINT('',#34677);
#7352=VERTEX_POINT('',#34679);
#7353=VERTEX_POINT('',#34683);
#7354=VERTEX_POINT('',#34687);
#7355=VERTEX_POINT('',#34689);
#7356=VERTEX_POINT('',#34693);
#7357=VERTEX_POINT('',#34697);
#7358=VERTEX_POINT('',#34699);
#7359=VERTEX_POINT('',#34703);
#7360=VERTEX_POINT('',#34707);
#7361=VERTEX_POINT('',#34709);
#7362=VERTEX_POINT('',#34713);
#7363=VERTEX_POINT('',#34717);
#7364=VERTEX_POINT('',#34719);
#7365=VERTEX_POINT('',#34723);
#7366=VERTEX_POINT('',#34727);
#7367=VERTEX_POINT('',#34729);
#7368=VERTEX_POINT('',#34733);
#7369=VERTEX_POINT('',#34737);
#7370=VERTEX_POINT('',#34739);
#7371=VERTEX_POINT('',#34743);
#7372=VERTEX_POINT('',#34747);
#7373=VERTEX_POINT('',#34749);
#7374=VERTEX_POINT('',#34753);
#7375=VERTEX_POINT('',#34757);
#7376=VERTEX_POINT('',#34759);
#7377=VERTEX_POINT('',#34763);
#7378=VERTEX_POINT('',#34767);
#7379=VERTEX_POINT('',#34769);
#7380=VERTEX_POINT('',#34773);
#7381=VERTEX_POINT('',#34777);
#7382=VERTEX_POINT('',#34779);
#7383=VERTEX_POINT('',#34783);
#7384=VERTEX_POINT('',#34787);
#7385=VERTEX_POINT('',#34789);
#7386=VERTEX_POINT('',#34793);
#7387=VERTEX_POINT('',#34797);
#7388=VERTEX_POINT('',#34799);
#7389=VERTEX_POINT('',#34803);
#7390=VERTEX_POINT('',#34807);
#7391=VERTEX_POINT('',#34809);
#7392=VERTEX_POINT('',#34813);
#7393=VERTEX_POINT('',#34817);
#7394=VERTEX_POINT('',#34819);
#7395=VERTEX_POINT('',#34823);
#7396=VERTEX_POINT('',#34827);
#7397=VERTEX_POINT('',#34829);
#7398=VERTEX_POINT('',#34833);
#7399=VERTEX_POINT('',#34837);
#7400=VERTEX_POINT('',#34839);
#7401=VERTEX_POINT('',#34843);
#7402=VERTEX_POINT('',#34847);
#7403=VERTEX_POINT('',#34849);
#7404=VERTEX_POINT('',#34853);
#7405=VERTEX_POINT('',#34857);
#7406=VERTEX_POINT('',#34859);
#7407=VERTEX_POINT('',#34863);
#7408=VERTEX_POINT('',#34867);
#7409=VERTEX_POINT('',#34869);
#7410=VERTEX_POINT('',#34873);
#7411=VERTEX_POINT('',#34877);
#7412=VERTEX_POINT('',#34879);
#7413=VERTEX_POINT('',#34883);
#7414=VERTEX_POINT('',#34887);
#7415=VERTEX_POINT('',#34889);
#7416=VERTEX_POINT('',#34893);
#7417=VERTEX_POINT('',#34897);
#7418=VERTEX_POINT('',#34899);
#7419=VERTEX_POINT('',#34903);
#7420=VERTEX_POINT('',#34907);
#7421=VERTEX_POINT('',#34909);
#7422=VERTEX_POINT('',#34913);
#7423=VERTEX_POINT('',#34917);
#7424=VERTEX_POINT('',#34919);
#7425=VERTEX_POINT('',#34923);
#7426=VERTEX_POINT('',#34927);
#7427=VERTEX_POINT('',#34929);
#7428=VERTEX_POINT('',#34933);
#7429=VERTEX_POINT('',#34937);
#7430=VERTEX_POINT('',#34939);
#7431=VERTEX_POINT('',#34943);
#7432=VERTEX_POINT('',#34947);
#7433=VERTEX_POINT('',#34949);
#7434=VERTEX_POINT('',#34953);
#7435=VERTEX_POINT('',#34957);
#7436=VERTEX_POINT('',#34959);
#7437=VERTEX_POINT('',#34963);
#7438=VERTEX_POINT('',#34967);
#7439=VERTEX_POINT('',#34969);
#7440=VERTEX_POINT('',#34973);
#7441=VERTEX_POINT('',#34977);
#7442=VERTEX_POINT('',#34979);
#7443=VERTEX_POINT('',#34983);
#7444=VERTEX_POINT('',#34987);
#7445=VERTEX_POINT('',#34993);
#7446=VERTEX_POINT('',#34994);
#7447=VERTEX_POINT('',#34998);
#7448=VERTEX_POINT('',#35000);
#7449=VERTEX_POINT('',#35004);
#7450=VERTEX_POINT('',#35008);
#7451=VERTEX_POINT('',#35010);
#7452=VERTEX_POINT('',#35014);
#7453=VERTEX_POINT('',#35018);
#7454=VERTEX_POINT('',#35020);
#7455=VERTEX_POINT('',#35024);
#7456=VERTEX_POINT('',#35028);
#7457=VERTEX_POINT('',#35030);
#7458=VERTEX_POINT('',#35034);
#7459=VERTEX_POINT('',#35038);
#7460=VERTEX_POINT('',#35040);
#7461=VERTEX_POINT('',#35044);
#7462=VERTEX_POINT('',#35048);
#7463=VERTEX_POINT('',#35050);
#7464=VERTEX_POINT('',#35054);
#7465=VERTEX_POINT('',#35058);
#7466=VERTEX_POINT('',#35060);
#7467=VERTEX_POINT('',#35064);
#7468=VERTEX_POINT('',#35068);
#7469=VERTEX_POINT('',#35070);
#7470=VERTEX_POINT('',#35074);
#7471=VERTEX_POINT('',#35078);
#7472=VERTEX_POINT('',#35080);
#7473=VERTEX_POINT('',#35084);
#7474=VERTEX_POINT('',#35088);
#7475=VERTEX_POINT('',#35090);
#7476=VERTEX_POINT('',#35094);
#7477=VERTEX_POINT('',#35098);
#7478=VERTEX_POINT('',#35100);
#7479=VERTEX_POINT('',#35104);
#7480=VERTEX_POINT('',#35108);
#7481=VERTEX_POINT('',#35110);
#7482=VERTEX_POINT('',#35114);
#7483=VERTEX_POINT('',#35118);
#7484=VERTEX_POINT('',#35120);
#7485=VERTEX_POINT('',#35124);
#7486=VERTEX_POINT('',#35128);
#7487=VERTEX_POINT('',#35130);
#7488=VERTEX_POINT('',#35134);
#7489=VERTEX_POINT('',#35138);
#7490=VERTEX_POINT('',#35140);
#7491=VERTEX_POINT('',#35144);
#7492=VERTEX_POINT('',#35148);
#7493=VERTEX_POINT('',#35150);
#7494=VERTEX_POINT('',#35154);
#7495=VERTEX_POINT('',#35158);
#7496=VERTEX_POINT('',#35160);
#7497=VERTEX_POINT('',#35164);
#7498=VERTEX_POINT('',#35168);
#7499=VERTEX_POINT('',#35170);
#7500=VERTEX_POINT('',#35174);
#7501=VERTEX_POINT('',#35178);
#7502=VERTEX_POINT('',#35180);
#7503=VERTEX_POINT('',#35184);
#7504=VERTEX_POINT('',#35188);
#7505=VERTEX_POINT('',#35190);
#7506=VERTEX_POINT('',#35194);
#7507=VERTEX_POINT('',#35198);
#7508=VERTEX_POINT('',#35200);
#7509=VERTEX_POINT('',#35204);
#7510=VERTEX_POINT('',#35208);
#7511=VERTEX_POINT('',#35210);
#7512=VERTEX_POINT('',#35214);
#7513=VERTEX_POINT('',#35218);
#7514=VERTEX_POINT('',#35220);
#7515=VERTEX_POINT('',#35224);
#7516=VERTEX_POINT('',#35228);
#7517=VERTEX_POINT('',#35230);
#7518=VERTEX_POINT('',#35234);
#7519=VERTEX_POINT('',#35238);
#7520=VERTEX_POINT('',#35240);
#7521=VERTEX_POINT('',#35244);
#7522=VERTEX_POINT('',#35248);
#7523=VERTEX_POINT('',#35250);
#7524=VERTEX_POINT('',#35254);
#7525=VERTEX_POINT('',#35258);
#7526=VERTEX_POINT('',#35260);
#7527=VERTEX_POINT('',#35264);
#7528=VERTEX_POINT('',#35268);
#7529=VERTEX_POINT('',#35270);
#7530=VERTEX_POINT('',#35274);
#7531=VERTEX_POINT('',#35278);
#7532=VERTEX_POINT('',#35280);
#7533=VERTEX_POINT('',#35284);
#7534=VERTEX_POINT('',#35288);
#7535=VERTEX_POINT('',#35290);
#7536=VERTEX_POINT('',#35294);
#7537=VERTEX_POINT('',#35298);
#7538=VERTEX_POINT('',#35300);
#7539=VERTEX_POINT('',#35304);
#7540=VERTEX_POINT('',#35308);
#7541=VERTEX_POINT('',#35310);
#7542=VERTEX_POINT('',#35314);
#7543=VERTEX_POINT('',#35318);
#7544=VERTEX_POINT('',#35320);
#7545=VERTEX_POINT('',#35324);
#7546=VERTEX_POINT('',#35328);
#7547=VERTEX_POINT('',#35330);
#7548=VERTEX_POINT('',#35334);
#7549=VERTEX_POINT('',#35338);
#7550=VERTEX_POINT('',#35340);
#7551=VERTEX_POINT('',#35344);
#7552=VERTEX_POINT('',#35348);
#7553=VERTEX_POINT('',#35350);
#7554=VERTEX_POINT('',#35354);
#7555=VERTEX_POINT('',#35358);
#7556=VERTEX_POINT('',#35360);
#7557=VERTEX_POINT('',#35364);
#7558=VERTEX_POINT('',#35368);
#7559=VERTEX_POINT('',#35370);
#7560=VERTEX_POINT('',#35374);
#7561=VERTEX_POINT('',#35378);
#7562=VERTEX_POINT('',#35380);
#7563=VERTEX_POINT('',#35384);
#7564=VERTEX_POINT('',#35387);
#7565=VERTEX_POINT('',#35391);
#7566=VERTEX_POINT('',#35395);
#7567=VERTEX_POINT('',#35397);
#7568=VERTEX_POINT('',#35401);
#7569=VERTEX_POINT('',#35405);
#7570=VERTEX_POINT('',#35407);
#7571=VERTEX_POINT('',#35411);
#7572=VERTEX_POINT('',#35415);
#7573=VERTEX_POINT('',#35417);
#7574=VERTEX_POINT('',#35421);
#7575=VERTEX_POINT('',#35425);
#7576=VERTEX_POINT('',#35427);
#7577=VERTEX_POINT('',#35431);
#7578=VERTEX_POINT('',#35435);
#7579=VERTEX_POINT('',#35437);
#7580=VERTEX_POINT('',#35441);
#7581=VERTEX_POINT('',#35445);
#7582=VERTEX_POINT('',#35447);
#7583=VERTEX_POINT('',#35451);
#7584=VERTEX_POINT('',#35455);
#7585=VERTEX_POINT('',#35457);
#7586=VERTEX_POINT('',#35461);
#7587=VERTEX_POINT('',#35465);
#7588=VERTEX_POINT('',#35467);
#7589=VERTEX_POINT('',#35471);
#7590=VERTEX_POINT('',#35475);
#7591=VERTEX_POINT('',#35477);
#7592=VERTEX_POINT('',#35481);
#7593=VERTEX_POINT('',#35485);
#7594=VERTEX_POINT('',#35487);
#7595=VERTEX_POINT('',#35491);
#7596=VERTEX_POINT('',#35495);
#7597=VERTEX_POINT('',#35497);
#7598=VERTEX_POINT('',#35501);
#7599=VERTEX_POINT('',#35505);
#7600=VERTEX_POINT('',#35507);
#7601=VERTEX_POINT('',#35511);
#7602=VERTEX_POINT('',#35515);
#7603=VERTEX_POINT('',#35517);
#7604=VERTEX_POINT('',#35521);
#7605=VERTEX_POINT('',#35525);
#7606=VERTEX_POINT('',#35527);
#7607=VERTEX_POINT('',#35531);
#7608=VERTEX_POINT('',#35535);
#7609=VERTEX_POINT('',#35537);
#7610=VERTEX_POINT('',#35541);
#7611=VERTEX_POINT('',#35545);
#7612=VERTEX_POINT('',#35547);
#7613=VERTEX_POINT('',#35551);
#7614=VERTEX_POINT('',#35555);
#7615=VERTEX_POINT('',#35557);
#7616=VERTEX_POINT('',#35561);
#7617=VERTEX_POINT('',#35565);
#7618=VERTEX_POINT('',#35567);
#7619=VERTEX_POINT('',#35571);
#7620=VERTEX_POINT('',#35575);
#7621=VERTEX_POINT('',#35577);
#7622=VERTEX_POINT('',#35581);
#7623=VERTEX_POINT('',#35585);
#7624=VERTEX_POINT('',#35587);
#7625=VERTEX_POINT('',#35591);
#7626=VERTEX_POINT('',#35595);
#7627=VERTEX_POINT('',#35597);
#7628=VERTEX_POINT('',#35601);
#7629=VERTEX_POINT('',#35605);
#7630=VERTEX_POINT('',#35607);
#7631=VERTEX_POINT('',#35611);
#7632=VERTEX_POINT('',#35615);
#7633=VERTEX_POINT('',#35617);
#7634=VERTEX_POINT('',#35621);
#7635=VERTEX_POINT('',#35625);
#7636=VERTEX_POINT('',#35627);
#7637=VERTEX_POINT('',#35631);
#7638=VERTEX_POINT('',#35635);
#7639=VERTEX_POINT('',#35637);
#7640=VERTEX_POINT('',#35641);
#7641=VERTEX_POINT('',#35645);
#7642=VERTEX_POINT('',#35647);
#7643=VERTEX_POINT('',#35651);
#7644=VERTEX_POINT('',#35655);
#7645=VERTEX_POINT('',#35657);
#7646=VERTEX_POINT('',#35661);
#7647=VERTEX_POINT('',#35665);
#7648=VERTEX_POINT('',#35667);
#7649=VERTEX_POINT('',#35671);
#7650=VERTEX_POINT('',#35675);
#7651=VERTEX_POINT('',#35677);
#7652=VERTEX_POINT('',#35681);
#7653=VERTEX_POINT('',#35685);
#7654=VERTEX_POINT('',#35687);
#7655=VERTEX_POINT('',#35691);
#7656=VERTEX_POINT('',#35695);
#7657=VERTEX_POINT('',#35697);
#7658=VERTEX_POINT('',#35701);
#7659=VERTEX_POINT('',#35705);
#7660=VERTEX_POINT('',#35707);
#7661=VERTEX_POINT('',#35711);
#7662=VERTEX_POINT('',#35715);
#7663=VERTEX_POINT('',#35717);
#7664=VERTEX_POINT('',#35721);
#7665=VERTEX_POINT('',#35725);
#7666=VERTEX_POINT('',#35727);
#7667=VERTEX_POINT('',#35731);
#7668=VERTEX_POINT('',#35735);
#7669=VERTEX_POINT('',#35737);
#7670=VERTEX_POINT('',#35741);
#7671=VERTEX_POINT('',#35745);
#7672=VERTEX_POINT('',#35747);
#7673=VERTEX_POINT('',#35751);
#7674=VERTEX_POINT('',#35755);
#7675=VERTEX_POINT('',#35757);
#7676=VERTEX_POINT('',#35761);
#7677=VERTEX_POINT('',#35765);
#7678=VERTEX_POINT('',#36238);
#7679=VERTEX_POINT('',#36239);
#7680=VERTEX_POINT('',#36241);
#7681=VERTEX_POINT('',#36252);
#7682=VERTEX_POINT('',#36254);
#7683=VERTEX_POINT('',#36265);
#7684=VERTEX_POINT('',#36267);
#7685=VERTEX_POINT('',#36269);
#7686=VERTEX_POINT('',#36272);
#7687=VERTEX_POINT('',#36274);
#7688=VERTEX_POINT('',#36285);
#7689=VERTEX_POINT('',#36298);
#7690=VERTEX_POINT('',#36302);
#7691=VERTEX_POINT('',#36304);
#7692=VERTEX_POINT('',#36319);
#7693=VERTEX_POINT('',#36321);
#7694=VERTEX_POINT('',#36325);
#7695=VERTEX_POINT('',#36326);
#7696=VERTEX_POINT('',#36329);
#7697=VERTEX_POINT('',#36333);
#7698=VERTEX_POINT('',#36334);
#7699=VERTEX_POINT('',#36337);
#7700=VERTEX_POINT('',#36339);
#7701=VERTEX_POINT('',#36345);
#7702=VERTEX_POINT('',#36346);
#7703=VERTEX_POINT('',#36351);
#7704=VERTEX_POINT('',#36352);
#7705=VERTEX_POINT('',#36355);
#7706=VERTEX_POINT('',#36357);
#7707=VERTEX_POINT('',#36363);
#7708=VERTEX_POINT('',#36364);
#7709=VERTEX_POINT('',#36369);
#7710=VERTEX_POINT('',#36370);
#7711=VERTEX_POINT('',#36373);
#7712=VERTEX_POINT('',#36375);
#7713=VERTEX_POINT('',#36381);
#7714=VERTEX_POINT('',#36382);
#7715=VERTEX_POINT('',#36387);
#7716=VERTEX_POINT('',#36388);
#7717=VERTEX_POINT('',#36391);
#7718=VERTEX_POINT('',#36393);
#7719=VERTEX_POINT('',#36399);
#7720=VERTEX_POINT('',#36400);
#7721=VERTEX_POINT('',#36405);
#7722=VERTEX_POINT('',#36406);
#7723=VERTEX_POINT('',#36409);
#7724=VERTEX_POINT('',#36411);
#7725=VERTEX_POINT('',#36417);
#7726=VERTEX_POINT('',#36418);
#7727=VERTEX_POINT('',#36423);
#7728=VERTEX_POINT('',#36424);
#7729=VERTEX_POINT('',#36427);
#7730=VERTEX_POINT('',#36429);
#7731=VERTEX_POINT('',#36435);
#7732=VERTEX_POINT('',#36436);
#7733=VERTEX_POINT('',#36441);
#7734=VERTEX_POINT('',#36442);
#7735=VERTEX_POINT('',#36445);
#7736=VERTEX_POINT('',#36447);
#7737=VERTEX_POINT('',#36453);
#7738=VERTEX_POINT('',#36454);
#7739=VERTEX_POINT('',#36459);
#7740=VERTEX_POINT('',#36460);
#7741=VERTEX_POINT('',#36463);
#7742=VERTEX_POINT('',#36465);
#7743=VERTEX_POINT('',#36471);
#7744=VERTEX_POINT('',#36472);
#7745=VERTEX_POINT('',#36477);
#7746=VERTEX_POINT('',#36478);
#7747=VERTEX_POINT('',#36481);
#7748=VERTEX_POINT('',#36483);
#7749=VERTEX_POINT('',#36489);
#7750=VERTEX_POINT('',#36490);
#7751=VERTEX_POINT('',#36495);
#7752=VERTEX_POINT('',#36496);
#7753=VERTEX_POINT('',#36499);
#7754=VERTEX_POINT('',#36501);
#7755=VERTEX_POINT('',#36507);
#7756=VERTEX_POINT('',#36508);
#7757=VERTEX_POINT('',#36513);
#7758=VERTEX_POINT('',#36514);
#7759=VERTEX_POINT('',#36517);
#7760=VERTEX_POINT('',#36519);
#7761=VERTEX_POINT('',#36525);
#7762=VERTEX_POINT('',#36526);
#7763=VERTEX_POINT('',#36531);
#7764=VERTEX_POINT('',#36532);
#7765=VERTEX_POINT('',#36535);
#7766=VERTEX_POINT('',#36537);
#7767=VERTEX_POINT('',#36543);
#7768=VERTEX_POINT('',#36544);
#7769=VERTEX_POINT('',#36549);
#7770=VERTEX_POINT('',#36550);
#7771=VERTEX_POINT('',#36553);
#7772=VERTEX_POINT('',#36555);
#7773=VERTEX_POINT('',#36561);
#7774=VERTEX_POINT('',#36565);
#7775=VERTEX_POINT('',#36566);
#7776=VERTEX_POINT('',#36570);
#7777=VERTEX_POINT('',#36572);
#7778=VERTEX_POINT('',#36576);
#7779=VERTEX_POINT('',#36580);
#7780=VERTEX_POINT('',#36582);
#7781=VERTEX_POINT('',#36586);
#7782=VERTEX_POINT('',#36590);
#7783=VERTEX_POINT('',#36592);
#7784=VERTEX_POINT('',#36596);
#7785=VERTEX_POINT('',#36600);
#7786=VERTEX_POINT('',#36602);
#7787=VERTEX_POINT('',#36606);
#7788=VERTEX_POINT('',#36610);
#7789=VERTEX_POINT('',#36612);
#7790=VERTEX_POINT('',#36616);
#7791=VERTEX_POINT('',#36620);
#7792=VERTEX_POINT('',#36622);
#7793=VERTEX_POINT('',#36626);
#7794=VERTEX_POINT('',#36630);
#7795=VERTEX_POINT('',#36632);
#7796=VERTEX_POINT('',#36636);
#7797=VERTEX_POINT('',#36640);
#7798=VERTEX_POINT('',#36642);
#7799=VERTEX_POINT('',#36646);
#7800=VERTEX_POINT('',#36650);
#7801=VERTEX_POINT('',#36652);
#7802=VERTEX_POINT('',#36656);
#7803=VERTEX_POINT('',#36660);
#7804=VERTEX_POINT('',#36662);
#7805=VERTEX_POINT('',#36666);
#7806=VERTEX_POINT('',#36670);
#7807=VERTEX_POINT('',#36672);
#7808=VERTEX_POINT('',#36676);
#7809=VERTEX_POINT('',#36680);
#7810=VERTEX_POINT('',#36682);
#7811=VERTEX_POINT('',#36686);
#7812=VERTEX_POINT('',#36690);
#7813=VERTEX_POINT('',#36692);
#7814=VERTEX_POINT('',#36696);
#7815=VERTEX_POINT('',#36700);
#7816=VERTEX_POINT('',#36702);
#7817=VERTEX_POINT('',#36706);
#7818=VERTEX_POINT('',#36710);
#7819=VERTEX_POINT('',#36712);
#7820=VERTEX_POINT('',#36716);
#7821=VERTEX_POINT('',#36720);
#7822=VERTEX_POINT('',#36722);
#7823=VERTEX_POINT('',#36726);
#7824=VERTEX_POINT('',#36730);
#7825=VERTEX_POINT('',#36732);
#7826=VERTEX_POINT('',#36736);
#7827=VERTEX_POINT('',#36740);
#7828=VERTEX_POINT('',#36742);
#7829=VERTEX_POINT('',#36746);
#7830=VERTEX_POINT('',#36750);
#7831=VERTEX_POINT('',#36752);
#7832=VERTEX_POINT('',#36756);
#7833=VERTEX_POINT('',#36760);
#7834=VERTEX_POINT('',#36762);
#7835=VERTEX_POINT('',#36766);
#7836=VERTEX_POINT('',#36770);
#7837=VERTEX_POINT('',#36772);
#7838=VERTEX_POINT('',#36776);
#7839=VERTEX_POINT('',#36780);
#7840=VERTEX_POINT('',#36782);
#7841=VERTEX_POINT('',#36786);
#7842=VERTEX_POINT('',#36790);
#7843=VERTEX_POINT('',#36792);
#7844=VERTEX_POINT('',#36796);
#7845=VERTEX_POINT('',#36800);
#7846=VERTEX_POINT('',#36802);
#7847=VERTEX_POINT('',#36806);
#7848=VERTEX_POINT('',#36810);
#7849=VERTEX_POINT('',#36812);
#7850=VERTEX_POINT('',#36816);
#7851=VERTEX_POINT('',#36820);
#7852=VERTEX_POINT('',#36822);
#7853=VERTEX_POINT('',#36826);
#7854=VERTEX_POINT('',#36830);
#7855=VERTEX_POINT('',#36832);
#7856=VERTEX_POINT('',#36836);
#7857=VERTEX_POINT('',#36840);
#7858=VERTEX_POINT('',#36842);
#7859=VERTEX_POINT('',#36846);
#7860=VERTEX_POINT('',#36850);
#7861=VERTEX_POINT('',#36852);
#7862=VERTEX_POINT('',#36856);
#7863=VERTEX_POINT('',#36860);
#7864=VERTEX_POINT('',#36862);
#7865=VERTEX_POINT('',#36866);
#7866=VERTEX_POINT('',#36870);
#7867=VERTEX_POINT('',#36872);
#7868=VERTEX_POINT('',#36876);
#7869=VERTEX_POINT('',#36880);
#7870=VERTEX_POINT('',#36882);
#7871=VERTEX_POINT('',#36886);
#7872=VERTEX_POINT('',#36890);
#7873=VERTEX_POINT('',#36892);
#7874=VERTEX_POINT('',#36896);
#7875=VERTEX_POINT('',#36900);
#7876=VERTEX_POINT('',#36902);
#7877=VERTEX_POINT('',#36906);
#7878=VERTEX_POINT('',#36910);
#7879=VERTEX_POINT('',#36912);
#7880=VERTEX_POINT('',#36916);
#7881=VERTEX_POINT('',#36920);
#7882=VERTEX_POINT('',#36922);
#7883=VERTEX_POINT('',#36926);
#7884=VERTEX_POINT('',#36930);
#7885=VERTEX_POINT('',#36932);
#7886=VERTEX_POINT('',#36936);
#7887=VERTEX_POINT('',#36940);
#7888=VERTEX_POINT('',#36942);
#7889=VERTEX_POINT('',#36946);
#7890=VERTEX_POINT('',#36950);
#7891=VERTEX_POINT('',#36952);
#7892=VERTEX_POINT('',#36956);
#7893=VERTEX_POINT('',#36959);
#7894=VERTEX_POINT('',#36963);
#7895=VERTEX_POINT('',#36967);
#7896=VERTEX_POINT('',#36969);
#7897=VERTEX_POINT('',#36973);
#7898=VERTEX_POINT('',#36977);
#7899=VERTEX_POINT('',#36979);
#7900=VERTEX_POINT('',#36983);
#7901=VERTEX_POINT('',#36987);
#7902=VERTEX_POINT('',#36989);
#7903=VERTEX_POINT('',#36993);
#7904=VERTEX_POINT('',#36997);
#7905=VERTEX_POINT('',#36999);
#7906=VERTEX_POINT('',#37003);
#7907=VERTEX_POINT('',#37007);
#7908=VERTEX_POINT('',#37009);
#7909=VERTEX_POINT('',#37013);
#7910=VERTEX_POINT('',#37017);
#7911=VERTEX_POINT('',#37019);
#7912=VERTEX_POINT('',#37023);
#7913=VERTEX_POINT('',#37027);
#7914=VERTEX_POINT('',#37029);
#7915=VERTEX_POINT('',#37033);
#7916=VERTEX_POINT('',#37037);
#7917=VERTEX_POINT('',#37039);
#7918=VERTEX_POINT('',#37043);
#7919=VERTEX_POINT('',#37047);
#7920=VERTEX_POINT('',#37049);
#7921=VERTEX_POINT('',#37053);
#7922=VERTEX_POINT('',#37057);
#7923=VERTEX_POINT('',#37059);
#7924=VERTEX_POINT('',#37063);
#7925=VERTEX_POINT('',#37067);
#7926=VERTEX_POINT('',#37069);
#7927=VERTEX_POINT('',#37073);
#7928=VERTEX_POINT('',#37077);
#7929=VERTEX_POINT('',#37079);
#7930=VERTEX_POINT('',#37083);
#7931=VERTEX_POINT('',#37087);
#7932=VERTEX_POINT('',#37089);
#7933=VERTEX_POINT('',#37093);
#7934=VERTEX_POINT('',#37097);
#7935=VERTEX_POINT('',#37099);
#7936=VERTEX_POINT('',#37103);
#7937=VERTEX_POINT('',#37107);
#7938=VERTEX_POINT('',#37109);
#7939=VERTEX_POINT('',#37113);
#7940=VERTEX_POINT('',#37117);
#7941=VERTEX_POINT('',#37119);
#7942=VERTEX_POINT('',#37123);
#7943=VERTEX_POINT('',#37127);
#7944=VERTEX_POINT('',#37129);
#7945=VERTEX_POINT('',#37133);
#7946=VERTEX_POINT('',#37137);
#7947=VERTEX_POINT('',#37139);
#7948=VERTEX_POINT('',#37143);
#7949=VERTEX_POINT('',#37147);
#7950=VERTEX_POINT('',#37149);
#7951=VERTEX_POINT('',#37153);
#7952=VERTEX_POINT('',#37157);
#7953=VERTEX_POINT('',#37159);
#7954=VERTEX_POINT('',#37163);
#7955=VERTEX_POINT('',#37167);
#7956=VERTEX_POINT('',#37169);
#7957=VERTEX_POINT('',#37173);
#7958=VERTEX_POINT('',#37177);
#7959=VERTEX_POINT('',#37179);
#7960=VERTEX_POINT('',#37183);
#7961=VERTEX_POINT('',#37187);
#7962=VERTEX_POINT('',#37189);
#7963=VERTEX_POINT('',#37193);
#7964=VERTEX_POINT('',#37197);
#7965=VERTEX_POINT('',#37199);
#7966=VERTEX_POINT('',#37203);
#7967=VERTEX_POINT('',#37207);
#7968=VERTEX_POINT('',#37209);
#7969=VERTEX_POINT('',#37213);
#7970=VERTEX_POINT('',#37217);
#7971=VERTEX_POINT('',#37219);
#7972=VERTEX_POINT('',#37223);
#7973=VERTEX_POINT('',#37227);
#7974=VERTEX_POINT('',#37229);
#7975=VERTEX_POINT('',#37233);
#7976=VERTEX_POINT('',#37237);
#7977=VERTEX_POINT('',#37239);
#7978=VERTEX_POINT('',#37243);
#7979=VERTEX_POINT('',#37247);
#7980=VERTEX_POINT('',#37249);
#7981=VERTEX_POINT('',#37253);
#7982=VERTEX_POINT('',#37257);
#7983=VERTEX_POINT('',#37259);
#7984=VERTEX_POINT('',#37263);
#7985=VERTEX_POINT('',#37267);
#7986=VERTEX_POINT('',#37269);
#7987=VERTEX_POINT('',#37273);
#7988=VERTEX_POINT('',#37277);
#7989=VERTEX_POINT('',#37279);
#7990=VERTEX_POINT('',#37283);
#7991=VERTEX_POINT('',#37287);
#7992=VERTEX_POINT('',#37289);
#7993=VERTEX_POINT('',#37293);
#7994=VERTEX_POINT('',#37297);
#7995=VERTEX_POINT('',#37299);
#7996=VERTEX_POINT('',#37303);
#7997=VERTEX_POINT('',#37307);
#7998=VERTEX_POINT('',#37309);
#7999=VERTEX_POINT('',#37313);
#8000=VERTEX_POINT('',#37317);
#8001=VERTEX_POINT('',#37319);
#8002=VERTEX_POINT('',#37323);
#8003=VERTEX_POINT('',#37327);
#8004=VERTEX_POINT('',#37329);
#8005=VERTEX_POINT('',#37333);
#8006=VERTEX_POINT('',#37337);
#8007=VERTEX_POINT('',#37343);
#8008=VERTEX_POINT('',#37344);
#8009=VERTEX_POINT('',#37348);
#8010=VERTEX_POINT('',#37350);
#8011=VERTEX_POINT('',#37354);
#8012=VERTEX_POINT('',#37358);
#8013=VERTEX_POINT('',#37360);
#8014=VERTEX_POINT('',#37364);
#8015=VERTEX_POINT('',#37368);
#8016=VERTEX_POINT('',#37370);
#8017=VERTEX_POINT('',#37374);
#8018=VERTEX_POINT('',#37378);
#8019=VERTEX_POINT('',#37380);
#8020=VERTEX_POINT('',#37384);
#8021=VERTEX_POINT('',#37388);
#8022=VERTEX_POINT('',#37390);
#8023=VERTEX_POINT('',#37394);
#8024=VERTEX_POINT('',#37398);
#8025=VERTEX_POINT('',#37400);
#8026=VERTEX_POINT('',#37404);
#8027=VERTEX_POINT('',#37408);
#8028=VERTEX_POINT('',#37410);
#8029=VERTEX_POINT('',#37414);
#8030=VERTEX_POINT('',#37418);
#8031=VERTEX_POINT('',#37420);
#8032=VERTEX_POINT('',#37424);
#8033=VERTEX_POINT('',#37428);
#8034=VERTEX_POINT('',#37430);
#8035=VERTEX_POINT('',#37434);
#8036=VERTEX_POINT('',#37438);
#8037=VERTEX_POINT('',#37440);
#8038=VERTEX_POINT('',#37444);
#8039=VERTEX_POINT('',#37448);
#8040=VERTEX_POINT('',#37450);
#8041=VERTEX_POINT('',#37454);
#8042=VERTEX_POINT('',#37458);
#8043=VERTEX_POINT('',#37460);
#8044=VERTEX_POINT('',#37464);
#8045=VERTEX_POINT('',#37468);
#8046=VERTEX_POINT('',#37470);
#8047=VERTEX_POINT('',#37474);
#8048=VERTEX_POINT('',#37478);
#8049=VERTEX_POINT('',#37480);
#8050=VERTEX_POINT('',#37484);
#8051=VERTEX_POINT('',#37488);
#8052=VERTEX_POINT('',#37490);
#8053=VERTEX_POINT('',#37494);
#8054=VERTEX_POINT('',#37498);
#8055=VERTEX_POINT('',#37500);
#8056=VERTEX_POINT('',#37504);
#8057=VERTEX_POINT('',#37508);
#8058=VERTEX_POINT('',#37510);
#8059=VERTEX_POINT('',#37514);
#8060=VERTEX_POINT('',#37518);
#8061=VERTEX_POINT('',#37520);
#8062=VERTEX_POINT('',#37524);
#8063=VERTEX_POINT('',#37528);
#8064=VERTEX_POINT('',#37530);
#8065=VERTEX_POINT('',#37534);
#8066=VERTEX_POINT('',#37538);
#8067=VERTEX_POINT('',#37540);
#8068=VERTEX_POINT('',#37544);
#8069=VERTEX_POINT('',#37548);
#8070=VERTEX_POINT('',#37550);
#8071=VERTEX_POINT('',#37554);
#8072=VERTEX_POINT('',#37558);
#8073=VERTEX_POINT('',#37560);
#8074=VERTEX_POINT('',#37564);
#8075=VERTEX_POINT('',#37568);
#8076=VERTEX_POINT('',#37570);
#8077=VERTEX_POINT('',#37574);
#8078=VERTEX_POINT('',#37578);
#8079=VERTEX_POINT('',#37580);
#8080=VERTEX_POINT('',#37584);
#8081=VERTEX_POINT('',#37588);
#8082=VERTEX_POINT('',#37590);
#8083=VERTEX_POINT('',#37594);
#8084=VERTEX_POINT('',#37598);
#8085=VERTEX_POINT('',#37600);
#8086=VERTEX_POINT('',#37604);
#8087=VERTEX_POINT('',#37608);
#8088=VERTEX_POINT('',#37610);
#8089=VERTEX_POINT('',#37614);
#8090=VERTEX_POINT('',#37618);
#8091=VERTEX_POINT('',#37620);
#8092=VERTEX_POINT('',#37624);
#8093=VERTEX_POINT('',#37628);
#8094=VERTEX_POINT('',#37630);
#8095=VERTEX_POINT('',#37634);
#8096=VERTEX_POINT('',#37638);
#8097=VERTEX_POINT('',#37640);
#8098=VERTEX_POINT('',#37644);
#8099=VERTEX_POINT('',#37648);
#8100=VERTEX_POINT('',#37650);
#8101=VERTEX_POINT('',#37654);
#8102=VERTEX_POINT('',#37658);
#8103=VERTEX_POINT('',#37660);
#8104=VERTEX_POINT('',#37664);
#8105=VERTEX_POINT('',#37668);
#8106=VERTEX_POINT('',#37670);
#8107=VERTEX_POINT('',#37674);
#8108=VERTEX_POINT('',#37678);
#8109=VERTEX_POINT('',#37680);
#8110=VERTEX_POINT('',#37684);
#8111=VERTEX_POINT('',#37688);
#8112=VERTEX_POINT('',#37690);
#8113=VERTEX_POINT('',#37694);
#8114=VERTEX_POINT('',#37698);
#8115=VERTEX_POINT('',#37700);
#8116=VERTEX_POINT('',#37704);
#8117=VERTEX_POINT('',#37708);
#8118=VERTEX_POINT('',#37710);
#8119=VERTEX_POINT('',#37714);
#8120=VERTEX_POINT('',#37718);
#8121=VERTEX_POINT('',#37720);
#8122=VERTEX_POINT('',#37724);
#8123=VERTEX_POINT('',#37728);
#8124=VERTEX_POINT('',#37730);
#8125=VERTEX_POINT('',#37734);
#8126=VERTEX_POINT('',#37737);
#8127=VERTEX_POINT('',#37741);
#8128=VERTEX_POINT('',#37745);
#8129=VERTEX_POINT('',#37747);
#8130=VERTEX_POINT('',#37751);
#8131=VERTEX_POINT('',#37755);
#8132=VERTEX_POINT('',#37757);
#8133=VERTEX_POINT('',#37761);
#8134=VERTEX_POINT('',#37765);
#8135=VERTEX_POINT('',#37767);
#8136=VERTEX_POINT('',#37771);
#8137=VERTEX_POINT('',#37775);
#8138=VERTEX_POINT('',#37777);
#8139=VERTEX_POINT('',#37781);
#8140=VERTEX_POINT('',#37785);
#8141=VERTEX_POINT('',#37787);
#8142=VERTEX_POINT('',#37791);
#8143=VERTEX_POINT('',#37795);
#8144=VERTEX_POINT('',#37797);
#8145=VERTEX_POINT('',#37801);
#8146=VERTEX_POINT('',#37805);
#8147=VERTEX_POINT('',#37807);
#8148=VERTEX_POINT('',#37811);
#8149=VERTEX_POINT('',#37815);
#8150=VERTEX_POINT('',#37817);
#8151=VERTEX_POINT('',#37821);
#8152=VERTEX_POINT('',#37825);
#8153=VERTEX_POINT('',#37827);
#8154=VERTEX_POINT('',#37831);
#8155=VERTEX_POINT('',#37835);
#8156=VERTEX_POINT('',#37837);
#8157=VERTEX_POINT('',#37841);
#8158=VERTEX_POINT('',#37845);
#8159=VERTEX_POINT('',#37847);
#8160=VERTEX_POINT('',#37851);
#8161=VERTEX_POINT('',#37855);
#8162=VERTEX_POINT('',#37857);
#8163=VERTEX_POINT('',#37861);
#8164=VERTEX_POINT('',#37865);
#8165=VERTEX_POINT('',#37867);
#8166=VERTEX_POINT('',#37871);
#8167=VERTEX_POINT('',#37875);
#8168=VERTEX_POINT('',#37877);
#8169=VERTEX_POINT('',#37881);
#8170=VERTEX_POINT('',#37885);
#8171=VERTEX_POINT('',#37887);
#8172=VERTEX_POINT('',#37891);
#8173=VERTEX_POINT('',#37895);
#8174=VERTEX_POINT('',#37897);
#8175=VERTEX_POINT('',#37901);
#8176=VERTEX_POINT('',#37905);
#8177=VERTEX_POINT('',#37907);
#8178=VERTEX_POINT('',#37911);
#8179=VERTEX_POINT('',#37915);
#8180=VERTEX_POINT('',#37917);
#8181=VERTEX_POINT('',#37921);
#8182=VERTEX_POINT('',#37925);
#8183=VERTEX_POINT('',#37927);
#8184=VERTEX_POINT('',#37931);
#8185=VERTEX_POINT('',#37935);
#8186=VERTEX_POINT('',#37937);
#8187=VERTEX_POINT('',#37941);
#8188=VERTEX_POINT('',#37945);
#8189=VERTEX_POINT('',#37947);
#8190=VERTEX_POINT('',#37951);
#8191=VERTEX_POINT('',#37955);
#8192=VERTEX_POINT('',#37957);
#8193=VERTEX_POINT('',#37961);
#8194=VERTEX_POINT('',#37965);
#8195=VERTEX_POINT('',#37967);
#8196=VERTEX_POINT('',#37971);
#8197=VERTEX_POINT('',#37975);
#8198=VERTEX_POINT('',#37977);
#8199=VERTEX_POINT('',#37981);
#8200=VERTEX_POINT('',#37985);
#8201=VERTEX_POINT('',#37987);
#8202=VERTEX_POINT('',#37991);
#8203=VERTEX_POINT('',#37995);
#8204=VERTEX_POINT('',#37997);
#8205=VERTEX_POINT('',#38001);
#8206=VERTEX_POINT('',#38005);
#8207=VERTEX_POINT('',#38007);
#8208=VERTEX_POINT('',#38011);
#8209=VERTEX_POINT('',#38015);
#8210=VERTEX_POINT('',#38017);
#8211=VERTEX_POINT('',#38021);
#8212=VERTEX_POINT('',#38025);
#8213=VERTEX_POINT('',#38027);
#8214=VERTEX_POINT('',#38031);
#8215=VERTEX_POINT('',#38035);
#8216=VERTEX_POINT('',#38037);
#8217=VERTEX_POINT('',#38041);
#8218=VERTEX_POINT('',#38045);
#8219=VERTEX_POINT('',#38047);
#8220=VERTEX_POINT('',#38051);
#8221=VERTEX_POINT('',#38055);
#8222=VERTEX_POINT('',#38057);
#8223=VERTEX_POINT('',#38061);
#8224=VERTEX_POINT('',#38065);
#8225=VERTEX_POINT('',#38067);
#8226=VERTEX_POINT('',#38071);
#8227=VERTEX_POINT('',#38075);
#8228=VERTEX_POINT('',#38077);
#8229=VERTEX_POINT('',#38081);
#8230=VERTEX_POINT('',#38085);
#8231=VERTEX_POINT('',#38087);
#8232=VERTEX_POINT('',#38091);
#8233=VERTEX_POINT('',#38095);
#8234=VERTEX_POINT('',#38097);
#8235=VERTEX_POINT('',#38101);
#8236=VERTEX_POINT('',#38105);
#8237=VERTEX_POINT('',#38107);
#8238=VERTEX_POINT('',#38111);
#8239=VERTEX_POINT('',#38115);
#8240=VERTEX_POINT('',#38121);
#8241=EDGE_CURVE('',#6512,#6513,#5586,.T.);
#8242=EDGE_CURVE('',#6513,#6514,#3698,.T.);
#8243=EDGE_CURVE('',#6515,#6514,#5587,.T.);
#8244=EDGE_CURVE('',#6515,#6512,#3699,.T.);
#8245=EDGE_CURVE('',#6516,#6517,#5588,.T.);
#8246=EDGE_CURVE('',#6516,#6518,#3700,.T.);
#8247=EDGE_CURVE('',#6519,#6518,#5589,.T.);
#8248=EDGE_CURVE('',#6519,#6517,#3701,.T.);
#8249=EDGE_CURVE('',#6520,#6516,#3702,.T.);
#8250=EDGE_CURVE('',#6521,#6520,#3703,.T.);
#8251=EDGE_CURVE('',#6522,#6521,#3704,.T.);
#8252=EDGE_CURVE('',#6522,#6523,#3705,.T.);
#8253=EDGE_CURVE('',#6523,#6514,#3706,.T.);
#8254=EDGE_CURVE('',#6518,#6513,#3707,.T.);
#8255=EDGE_CURVE('',#6517,#6524,#3708,.T.);
#8256=EDGE_CURVE('',#6512,#6519,#3709,.T.);
#8257=EDGE_CURVE('',#6515,#6525,#3710,.T.);
#8258=EDGE_CURVE('',#6525,#6526,#3711,.T.);
#8259=EDGE_CURVE('',#6527,#6526,#3712,.T.);
#8260=EDGE_CURVE('',#6524,#6527,#3713,.T.);
#8261=EDGE_CURVE('',#6521,#6527,#5590,.T.);
#8262=EDGE_CURVE('',#6526,#6522,#5591,.T.);
#8263=EDGE_CURVE('',#6525,#6523,#5592,.T.);
#8264=EDGE_CURVE('',#6520,#6524,#5593,.T.);
#8265=EDGE_CURVE('',#6528,#6529,#5594,.T.);
#8266=EDGE_CURVE('',#6529,#6530,#3714,.T.);
#8267=EDGE_CURVE('',#6530,#6531,#5595,.T.);
#8268=EDGE_CURVE('',#6531,#6528,#3715,.T.);
#8269=EDGE_CURVE('',#6532,#6533,#5596,.T.);
#8270=EDGE_CURVE('',#6534,#6533,#3716,.T.);
#8271=EDGE_CURVE('',#6535,#6534,#5597,.T.);
#8272=EDGE_CURVE('',#6532,#6535,#3717,.T.);
#8273=EDGE_CURVE('',#6536,#6537,#5598,.T.);
#8274=EDGE_CURVE('',#6536,#6538,#3718,.T.);
#8275=EDGE_CURVE('',#6539,#6538,#5599,.T.);
#8276=EDGE_CURVE('',#6539,#6537,#3719,.T.);
#8277=EDGE_CURVE('',#6528,#6539,#3720,.T.);
#8278=EDGE_CURVE('',#6534,#6531,#3721,.T.);
#8279=EDGE_CURVE('',#6533,#6540,#3722,.T.);
#8280=EDGE_CURVE('',#6541,#6540,#3723,.T.);
#8281=EDGE_CURVE('',#6537,#6541,#3724,.T.);
#8282=EDGE_CURVE('',#6538,#6529,#3725,.T.);
#8283=EDGE_CURVE('',#6542,#6536,#3726,.T.);
#8284=EDGE_CURVE('',#6543,#6542,#3727,.T.);
#8285=EDGE_CURVE('',#6543,#6532,#3728,.T.);
#8286=EDGE_CURVE('',#6530,#6535,#3729,.T.);
#8287=EDGE_CURVE('',#6543,#6540,#5600,.T.);
#8288=EDGE_CURVE('',#6542,#6541,#5601,.T.);
#8289=EDGE_CURVE('',#6544,#6545,#3730,.T.);
#8290=EDGE_CURVE('',#6544,#6546,#3731,.T.);
#8291=EDGE_CURVE('',#6546,#6547,#3732,.T.);
#8292=EDGE_CURVE('',#6547,#6545,#3733,.T.);
#8293=EDGE_CURVE('',#6548,#6549,#3734,.T.);
#8294=EDGE_CURVE('',#6549,#6544,#3735,.T.);
#8295=EDGE_CURVE('',#6545,#6550,#3736,.T.);
#8296=EDGE_CURVE('',#6550,#6551,#3737,.T.);
#8297=EDGE_CURVE('',#6552,#6551,#3738,.T.);
#8298=EDGE_CURVE('',#6553,#6552,#3739,.T.);
#8299=EDGE_CURVE('',#6553,#6548,#3740,.T.);
#8300=EDGE_CURVE('',#6546,#6554,#3741,.T.);
#8301=EDGE_CURVE('',#6554,#6555,#3742,.T.);
#8302=EDGE_CURVE('',#6555,#6556,#3743,.T.);
#8303=EDGE_CURVE('',#6556,#6557,#3744,.T.);
#8304=EDGE_CURVE('',#6558,#6557,#3745,.T.);
#8305=EDGE_CURVE('',#6558,#6559,#3746,.T.);
#8306=EDGE_CURVE('',#6559,#6547,#3747,.T.);
#8307=EDGE_CURVE('',#6555,#6548,#5602,.T.);
#8308=EDGE_CURVE('',#6556,#6553,#5603,.T.);
#8309=EDGE_CURVE('',#6551,#6558,#5604,.T.);
#8310=EDGE_CURVE('',#6557,#6552,#5605,.T.);
#8311=EDGE_CURVE('',#6550,#6559,#5606,.T.);
#8312=EDGE_CURVE('',#6554,#6549,#5607,.T.);
#8313=EDGE_CURVE('',#6560,#6561,#3748,.T.);
#8314=EDGE_CURVE('',#6560,#6562,#3749,.T.);
#8315=EDGE_CURVE('',#6562,#6563,#3750,.T.);
#8316=EDGE_CURVE('',#6563,#6561,#3751,.T.);
#8317=EDGE_CURVE('',#6564,#6565,#3752,.T.);
#8318=EDGE_CURVE('',#6565,#6560,#3753,.T.);
#8319=EDGE_CURVE('',#6561,#6566,#3754,.T.);
#8320=EDGE_CURVE('',#6566,#6567,#3755,.T.);
#8321=EDGE_CURVE('',#6568,#6567,#3756,.T.);
#8322=EDGE_CURVE('',#6569,#6568,#3757,.T.);
#8323=EDGE_CURVE('',#6569,#6564,#3758,.T.);
#8324=EDGE_CURVE('',#6562,#6570,#3759,.T.);
#8325=EDGE_CURVE('',#6570,#6571,#3760,.T.);
#8326=EDGE_CURVE('',#6571,#6572,#3761,.T.);
#8327=EDGE_CURVE('',#6572,#6573,#3762,.T.);
#8328=EDGE_CURVE('',#6574,#6573,#3763,.T.);
#8329=EDGE_CURVE('',#6574,#6575,#3764,.T.);
#8330=EDGE_CURVE('',#6575,#6563,#3765,.T.);
#8331=EDGE_CURVE('',#6571,#6564,#5608,.T.);
#8332=EDGE_CURVE('',#6572,#6569,#5609,.T.);
#8333=EDGE_CURVE('',#6567,#6574,#5610,.T.);
#8334=EDGE_CURVE('',#6573,#6568,#5611,.T.);
#8335=EDGE_CURVE('',#6566,#6575,#5612,.T.);
#8336=EDGE_CURVE('',#6570,#6565,#5613,.T.);
#8337=EDGE_CURVE('',#6576,#6577,#5614,.T.);
#8338=EDGE_CURVE('',#6576,#6578,#3766,.T.);
#8339=EDGE_CURVE('',#6579,#6578,#5615,.T.);
#8340=EDGE_CURVE('',#6579,#6577,#3767,.T.);
#8341=EDGE_CURVE('',#6580,#6581,#5616,.T.);
#8342=EDGE_CURVE('',#6581,#6580,#3768,.T.);
#8343=EDGE_CURVE('',#6577,#6582,#3769,.T.);
#8344=EDGE_CURVE('',#6579,#6578,#3770,.T.);
#8345=EDGE_CURVE('',#6583,#6576,#3771,.T.);
#8346=EDGE_CURVE('',#6580,#6583,#3772,.T.);
#8347=EDGE_CURVE('',#6582,#6581,#3773,.T.);
#8348=EDGE_CURVE('',#6583,#6582,#5617,.T.);
#8349=EDGE_CURVE('',#6584,#6585,#5618,.T.);
#8350=EDGE_CURVE('',#6585,#6586,#3774,.T.);
#8351=EDGE_CURVE('',#6587,#6586,#5619,.T.);
#8352=EDGE_CURVE('',#6587,#6584,#3775,.T.);
#8353=EDGE_CURVE('',#6588,#6589,#5620,.T.);
#8354=EDGE_CURVE('',#6588,#6590,#3776,.T.);
#8355=EDGE_CURVE('',#6591,#6590,#5621,.T.);
#8356=EDGE_CURVE('',#6591,#6589,#3777,.T.);
#8357=EDGE_CURVE('',#6586,#6587,#3778,.T.);
#8358=EDGE_CURVE('',#6590,#6585,#3779,.T.);
#8359=EDGE_CURVE('',#6588,#6589,#3780,.T.);
#8360=EDGE_CURVE('',#6584,#6591,#3781,.T.);
#8361=EDGE_CURVE('',#6592,#6593,#3782,.T.);
#8362=EDGE_CURVE('',#6592,#6594,#3783,.T.);
#8363=EDGE_CURVE('',#6594,#6595,#3784,.T.);
#8364=EDGE_CURVE('',#6593,#6595,#3785,.T.);
#8365=EDGE_CURVE('',#6596,#6597,#3786,.T.);
#8366=EDGE_CURVE('',#6596,#6598,#3787,.T.);
#8367=EDGE_CURVE('',#6598,#6599,#3788,.T.);
#8368=EDGE_CURVE('',#6599,#6600,#3789,.T.);
#8369=EDGE_CURVE('',#6600,#6601,#3790,.T.);
#8370=EDGE_CURVE('',#6601,#6592,#3791,.T.);
#8371=EDGE_CURVE('',#6597,#6593,#3792,.T.);
#8372=EDGE_CURVE('',#6602,#6603,#3793,.T.);
#8373=EDGE_CURVE('',#6602,#6596,#3794,.T.);
#8374=EDGE_CURVE('',#6603,#6597,#3795,.T.);
#8375=EDGE_CURVE('',#6594,#6604,#3796,.T.);
#8376=EDGE_CURVE('',#6604,#6605,#3797,.T.);
#8377=EDGE_CURVE('',#6605,#6606,#3798,.T.);
#8378=EDGE_CURVE('',#6606,#6607,#3799,.T.);
#8379=EDGE_CURVE('',#6607,#6602,#3800,.T.);
#8380=EDGE_CURVE('',#6595,#6603,#3801,.T.);
#8381=EDGE_CURVE('',#6605,#6600,#5622,.T.);
#8382=EDGE_CURVE('',#6599,#6606,#5623,.T.);
#8383=EDGE_CURVE('',#6598,#6607,#5624,.T.);
#8384=EDGE_CURVE('',#6604,#6601,#5625,.T.);
#8385=EDGE_CURVE('',#6608,#6609,#3802,.T.);
#8386=EDGE_CURVE('',#6609,#6609,#5626,.T.);
#8387=EDGE_CURVE('',#6609,#6610,#3803,.T.);
#8388=EDGE_CURVE('',#6610,#6610,#907,.T.);
#8389=EDGE_CURVE('',#6611,#6611,#5627,.T.);
#8390=EDGE_CURVE('',#6611,#6612,#3804,.T.);
#8391=EDGE_CURVE('',#6612,#6612,#5628,.T.);
#8392=EDGE_CURVE('',#6613,#6614,#5629,.T.);
#8393=EDGE_CURVE('',#6614,#6613,#5630,.T.);
#8394=EDGE_CURVE('',#6614,#6615,#3805,.T.);
#8395=EDGE_CURVE('',#6615,#6615,#5631,.T.);
#8396=EDGE_CURVE('',#6616,#6616,#5632,.T.);
#8397=EDGE_CURVE('',#6616,#6611,#3806,.T.);
#8398=EDGE_CURVE('',#6617,#6617,#5633,.T.);
#8399=EDGE_CURVE('',#6617,#6613,#3807,.T.);
#8400=EDGE_CURVE('',#6618,#6619,#3808,.T.);
#8401=EDGE_CURVE('',#6620,#6619,#186,.T.);
#8402=EDGE_CURVE('',#6620,#6621,#3809,.T.);
#8403=EDGE_CURVE('',#6621,#6618,#187,.T.);
#8404=EDGE_CURVE('',#6622,#6623,#3810,.T.);
#8405=EDGE_CURVE('',#6619,#6623,#188,.T.);
#8406=EDGE_CURVE('',#6618,#6622,#189,.T.);
#8407=EDGE_CURVE('',#6624,#6625,#3811,.T.);
#8408=EDGE_CURVE('',#6623,#6625,#190,.T.);
#8409=EDGE_CURVE('',#6622,#6624,#191,.T.);
#8410=EDGE_CURVE('',#6626,#6627,#3812,.T.);
#8411=EDGE_CURVE('',#6625,#6627,#192,.T.);
#8412=EDGE_CURVE('',#6624,#6626,#193,.T.);
#8413=EDGE_CURVE('',#6628,#6629,#3813,.T.);
#8414=EDGE_CURVE('',#6627,#6629,#194,.T.);
#8415=EDGE_CURVE('',#6626,#6628,#195,.T.);
#8416=EDGE_CURVE('',#6630,#6631,#3814,.T.);
#8417=EDGE_CURVE('',#6629,#6631,#196,.T.);
#8418=EDGE_CURVE('',#6628,#6630,#197,.T.);
#8419=EDGE_CURVE('',#6632,#6633,#3815,.T.);
#8420=EDGE_CURVE('',#6631,#6633,#198,.T.);
#8421=EDGE_CURVE('',#6630,#6632,#199,.T.);
#8422=EDGE_CURVE('',#6634,#6635,#3816,.T.);
#8423=EDGE_CURVE('',#6633,#6635,#200,.T.);
#8424=EDGE_CURVE('',#6632,#6634,#201,.T.);
#8425=EDGE_CURVE('',#6636,#6637,#3817,.T.);
#8426=EDGE_CURVE('',#6635,#6637,#202,.T.);
#8427=EDGE_CURVE('',#6634,#6636,#203,.T.);
#8428=EDGE_CURVE('',#6638,#6639,#3818,.T.);
#8429=EDGE_CURVE('',#6637,#6639,#204,.T.);
#8430=EDGE_CURVE('',#6636,#6638,#205,.T.);
#8431=EDGE_CURVE('',#6640,#6641,#3819,.T.);
#8432=EDGE_CURVE('',#6639,#6641,#206,.T.);
#8433=EDGE_CURVE('',#6638,#6640,#207,.T.);
#8434=EDGE_CURVE('',#6642,#6643,#3820,.T.);
#8435=EDGE_CURVE('',#6641,#6643,#208,.T.);
#8436=EDGE_CURVE('',#6640,#6642,#209,.T.);
#8437=EDGE_CURVE('',#6644,#6645,#3821,.T.);
#8438=EDGE_CURVE('',#6643,#6645,#210,.T.);
#8439=EDGE_CURVE('',#6642,#6644,#211,.T.);
#8440=EDGE_CURVE('',#6646,#6647,#3822,.T.);
#8441=EDGE_CURVE('',#6645,#6647,#212,.T.);
#8442=EDGE_CURVE('',#6644,#6646,#213,.T.);
#8443=EDGE_CURVE('',#6648,#6649,#3823,.T.);
#8444=EDGE_CURVE('',#6647,#6649,#214,.T.);
#8445=EDGE_CURVE('',#6646,#6648,#215,.T.);
#8446=EDGE_CURVE('',#6650,#6651,#3824,.T.);
#8447=EDGE_CURVE('',#6649,#6651,#216,.T.);
#8448=EDGE_CURVE('',#6648,#6650,#217,.T.);
#8449=EDGE_CURVE('',#6652,#6653,#3825,.T.);
#8450=EDGE_CURVE('',#6651,#6653,#218,.T.);
#8451=EDGE_CURVE('',#6650,#6652,#219,.T.);
#8452=EDGE_CURVE('',#6654,#6655,#3826,.T.);
#8453=EDGE_CURVE('',#6653,#6655,#220,.T.);
#8454=EDGE_CURVE('',#6652,#6654,#221,.T.);
#8455=EDGE_CURVE('',#6656,#6657,#3827,.T.);
#8456=EDGE_CURVE('',#6655,#6657,#222,.T.);
#8457=EDGE_CURVE('',#6654,#6656,#223,.T.);
#8458=EDGE_CURVE('',#6658,#6659,#3828,.T.);
#8459=EDGE_CURVE('',#6657,#6659,#224,.T.);
#8460=EDGE_CURVE('',#6656,#6658,#225,.T.);
#8461=EDGE_CURVE('',#6660,#6661,#3829,.T.);
#8462=EDGE_CURVE('',#6659,#6661,#226,.T.);
#8463=EDGE_CURVE('',#6658,#6660,#227,.T.);
#8464=EDGE_CURVE('',#6662,#6663,#3830,.T.);
#8465=EDGE_CURVE('',#6661,#6663,#228,.T.);
#8466=EDGE_CURVE('',#6660,#6662,#229,.T.);
#8467=EDGE_CURVE('',#6664,#6665,#3831,.T.);
#8468=EDGE_CURVE('',#6663,#6665,#230,.T.);
#8469=EDGE_CURVE('',#6662,#6664,#231,.T.);
#8470=EDGE_CURVE('',#6666,#6667,#3832,.T.);
#8471=EDGE_CURVE('',#6665,#6667,#232,.T.);
#8472=EDGE_CURVE('',#6664,#6666,#233,.T.);
#8473=EDGE_CURVE('',#6668,#6669,#3833,.T.);
#8474=EDGE_CURVE('',#6668,#6670,#234,.T.);
#8475=EDGE_CURVE('',#6671,#6670,#5634,.T.);
#8476=EDGE_CURVE('',#6669,#6671,#235,.T.);
#8477=EDGE_CURVE('',#6672,#6673,#3834,.T.);
#8478=EDGE_CURVE('',#6673,#6674,#5635,.T.);
#8479=EDGE_CURVE('',#6674,#6672,#908,.T.);
#8480=EDGE_CURVE('',#6675,#6676,#3835,.T.);
#8481=EDGE_CURVE('',#6677,#6676,#909,.F.);
#8482=EDGE_CURVE('',#6677,#6674,#3836,.T.);
#8483=EDGE_CURVE('',#6674,#6673,#5636,.T.);
#8484=EDGE_CURVE('',#6672,#6675,#910,.T.);
#8485=EDGE_CURVE('',#6678,#6679,#3837,.T.);
#8486=EDGE_CURVE('',#6676,#6679,#911,.F.);
#8487=EDGE_CURVE('',#6675,#6678,#912,.T.);
#8488=EDGE_CURVE('',#6680,#6681,#3838,.T.);
#8489=EDGE_CURVE('',#6679,#6681,#913,.F.);
#8490=EDGE_CURVE('',#6678,#6680,#914,.T.);
#8491=EDGE_CURVE('',#6682,#6683,#3839,.T.);
#8492=EDGE_CURVE('',#6681,#6683,#915,.F.);
#8493=EDGE_CURVE('',#6680,#6682,#916,.T.);
#8494=EDGE_CURVE('',#6684,#6685,#3840,.T.);
#8495=EDGE_CURVE('',#6683,#6685,#917,.F.);
#8496=EDGE_CURVE('',#6682,#6684,#918,.T.);
#8497=EDGE_CURVE('',#6686,#6687,#3841,.T.);
#8498=EDGE_CURVE('',#6685,#6687,#919,.F.);
#8499=EDGE_CURVE('',#6684,#6686,#920,.T.);
#8500=EDGE_CURVE('',#6688,#6689,#3842,.T.);
#8501=EDGE_CURVE('',#6687,#6689,#921,.F.);
#8502=EDGE_CURVE('',#6686,#6688,#922,.T.);
#8503=EDGE_CURVE('',#6690,#6691,#3843,.T.);
#8504=EDGE_CURVE('',#6689,#6691,#923,.F.);
#8505=EDGE_CURVE('',#6688,#6690,#924,.T.);
#8506=EDGE_CURVE('',#6692,#6693,#3844,.T.);
#8507=EDGE_CURVE('',#6691,#6693,#925,.F.);
#8508=EDGE_CURVE('',#6690,#6692,#926,.T.);
#8509=EDGE_CURVE('',#6694,#6695,#3845,.T.);
#8510=EDGE_CURVE('',#6693,#6695,#927,.F.);
#8511=EDGE_CURVE('',#6692,#6694,#928,.T.);
#8512=EDGE_CURVE('',#6696,#6697,#3846,.T.);
#8513=EDGE_CURVE('',#6695,#6697,#929,.F.);
#8514=EDGE_CURVE('',#6694,#6696,#930,.T.);
#8515=EDGE_CURVE('',#6698,#6699,#3847,.T.);
#8516=EDGE_CURVE('',#6697,#6699,#931,.F.);
#8517=EDGE_CURVE('',#6696,#6698,#932,.T.);
#8518=EDGE_CURVE('',#6700,#6701,#3848,.T.);
#8519=EDGE_CURVE('',#6699,#6701,#933,.F.);
#8520=EDGE_CURVE('',#6698,#6700,#934,.T.);
#8521=EDGE_CURVE('',#6702,#6703,#3849,.T.);
#8522=EDGE_CURVE('',#6701,#6703,#935,.F.);
#8523=EDGE_CURVE('',#6700,#6702,#936,.T.);
#8524=EDGE_CURVE('',#6704,#6705,#3850,.T.);
#8525=EDGE_CURVE('',#6703,#6705,#937,.F.);
#8526=EDGE_CURVE('',#6702,#6704,#938,.T.);
#8527=EDGE_CURVE('',#6706,#6707,#3851,.T.);
#8528=EDGE_CURVE('',#6705,#6707,#939,.F.);
#8529=EDGE_CURVE('',#6704,#6706,#940,.T.);
#8530=EDGE_CURVE('',#6708,#6709,#3852,.T.);
#8531=EDGE_CURVE('',#6707,#6709,#941,.F.);
#8532=EDGE_CURVE('',#6706,#6708,#942,.T.);
#8533=EDGE_CURVE('',#6710,#6711,#3853,.T.);
#8534=EDGE_CURVE('',#6709,#6711,#943,.F.);
#8535=EDGE_CURVE('',#6708,#6710,#944,.T.);
#8536=EDGE_CURVE('',#6712,#6713,#3854,.T.);
#8537=EDGE_CURVE('',#6711,#6713,#945,.F.);
#8538=EDGE_CURVE('',#6710,#6712,#946,.T.);
#8539=EDGE_CURVE('',#6714,#6715,#3855,.T.);
#8540=EDGE_CURVE('',#6713,#6715,#947,.F.);
#8541=EDGE_CURVE('',#6712,#6714,#948,.T.);
#8542=EDGE_CURVE('',#6716,#6717,#3856,.T.);
#8543=EDGE_CURVE('',#6715,#6717,#949,.F.);
#8544=EDGE_CURVE('',#6714,#6716,#950,.T.);
#8545=EDGE_CURVE('',#6718,#6719,#3857,.T.);
#8546=EDGE_CURVE('',#6717,#6719,#951,.F.);
#8547=EDGE_CURVE('',#6716,#6718,#952,.T.);
#8548=EDGE_CURVE('',#6720,#6721,#3858,.T.);
#8549=EDGE_CURVE('',#6719,#6721,#953,.F.);
#8550=EDGE_CURVE('',#6718,#6720,#954,.T.);
#8551=EDGE_CURVE('',#6722,#6723,#3859,.T.);
#8552=EDGE_CURVE('',#6722,#6724,#955,.T.);
#8553=EDGE_CURVE('',#6724,#6725,#5637,.T.);
#8554=EDGE_CURVE('',#6723,#6725,#956,.F.);
#8555=EDGE_CURVE('',#6673,#6726,#3860,.T.);
#8556=EDGE_CURVE('',#6726,#6726,#5638,.T.);
#8557=EDGE_CURVE('',#6727,#6727,#5639,.T.);
#8558=EDGE_CURVE('',#6727,#6728,#3861,.T.);
#8559=EDGE_CURVE('',#6729,#6728,#5640,.T.);
#8560=EDGE_CURVE('',#6730,#6729,#957,.T.);
#8561=EDGE_CURVE('',#6731,#6730,#5641,.T.);
#8562=EDGE_CURVE('',#6731,#6732,#3862,.T.);
#8563=EDGE_CURVE('',#6732,#6732,#5642,.T.);
#8564=EDGE_CURVE('',#6733,#6731,#5643,.T.);
#8565=EDGE_CURVE('',#6734,#6733,#958,.T.);
#8566=EDGE_CURVE('',#6728,#6734,#5644,.T.);
#8567=EDGE_CURVE('',#6735,#6735,#5645,.T.);
#8568=EDGE_CURVE('',#6735,#6736,#5646,.T.);
#8569=EDGE_CURVE('',#6736,#6736,#5647,.T.);
#8570=EDGE_CURVE('',#6737,#6737,#5648,.T.);
#8571=EDGE_CURVE('',#6737,#6738,#3863,.T.);
#8572=EDGE_CURVE('',#6738,#6739,#5649,.T.);
#8573=EDGE_CURVE('',#6740,#6739,#959,.T.);
#8574=EDGE_CURVE('',#6741,#6740,#5650,.T.);
#8575=EDGE_CURVE('',#6741,#6735,#3864,.T.);
#8576=EDGE_CURVE('',#6742,#6741,#5651,.T.);
#8577=EDGE_CURVE('',#6743,#6742,#960,.T.);
#8578=EDGE_CURVE('',#6743,#6738,#5652,.T.);
#8579=EDGE_CURVE('',#6744,#6744,#5653,.T.);
#8580=EDGE_CURVE('',#6744,#6745,#5654,.T.);
#8581=EDGE_CURVE('',#6745,#6745,#5655,.T.);
#8582=EDGE_CURVE('',#6746,#6746,#5656,.T.);
#8583=EDGE_CURVE('',#6746,#6744,#3865,.T.);
#8584=EDGE_CURVE('',#6747,#6747,#5657,.T.);
#8585=EDGE_CURVE('',#6747,#6748,#3866,.T.);
#8586=EDGE_CURVE('',#6748,#6748,#5658,.T.);
#8587=EDGE_CURVE('',#6721,#6723,#961,.F.);
#8588=EDGE_CURVE('',#6720,#6722,#962,.T.);
#8589=EDGE_CURVE('',#6724,#6671,#963,.T.);
#8590=EDGE_CURVE('',#6670,#6725,#964,.T.);
#8591=EDGE_CURVE('',#6733,#6743,#3867,.T.);
#8592=EDGE_CURVE('',#6734,#6742,#3868,.T.);
#8593=EDGE_CURVE('',#6729,#6740,#3869,.T.);
#8594=EDGE_CURVE('',#6730,#6739,#3870,.T.);
#8595=EDGE_CURVE('',#6674,#6620,#3871,.T.);
#8596=EDGE_CURVE('',#6621,#6677,#3872,.T.);
#8597=EDGE_CURVE('',#6667,#6669,#236,.T.);
#8598=EDGE_CURVE('',#6666,#6668,#237,.T.);
#8599=EDGE_CURVE('',#6749,#6749,#5659,.T.);
#8600=EDGE_CURVE('',#6749,#6750,#3873,.T.);
#8601=EDGE_CURVE('',#6750,#6750,#5660,.T.);
#8602=EDGE_CURVE('',#6751,#6751,#5661,.T.);
#8603=EDGE_CURVE('',#6751,#6752,#3874,.T.);
#8604=EDGE_CURVE('',#6752,#6752,#5662,.T.);
#8605=EDGE_CURVE('',#6753,#6753,#5663,.T.);
#8606=EDGE_CURVE('',#6753,#6754,#3875,.T.);
#8607=EDGE_CURVE('',#6754,#6754,#5664,.T.);
#8608=EDGE_CURVE('',#6755,#6755,#5665,.T.);
#8609=EDGE_CURVE('',#6755,#6756,#3876,.T.);
#8610=EDGE_CURVE('',#6756,#6756,#5666,.T.);
#8611=EDGE_CURVE('',#6757,#6758,#5667,.T.);
#8612=EDGE_CURVE('',#6758,#6757,#5668,.T.);
#8613=EDGE_CURVE('',#6758,#6759,#5669,.T.);
#8614=EDGE_CURVE('',#6759,#6759,#5670,.T.);
#8615=EDGE_CURVE('',#6760,#6760,#5671,.T.);
#8616=EDGE_CURVE('',#6760,#6761,#5672,.T.);
#8617=EDGE_CURVE('',#6761,#6761,#5673,.T.);
#8618=EDGE_CURVE('',#6761,#6762,#3877,.T.);
#8619=EDGE_CURVE('',#6762,#6762,#5674,.T.);
#8620=EDGE_CURVE('',#6757,#6760,#3878,.T.);
#8621=EDGE_CURVE('',#6763,#6763,#5675,.T.);
#8622=EDGE_CURVE('',#6763,#6764,#5676,.T.);
#8623=EDGE_CURVE('',#6764,#6764,#5677,.T.);
#8624=EDGE_CURVE('',#6764,#6765,#3879,.T.);
#8625=EDGE_CURVE('',#6765,#6765,#5678,.T.);
#8626=EDGE_CURVE('',#6765,#6766,#3880,.T.);
#8627=EDGE_CURVE('',#6766,#6766,#5679,.T.);
#8628=EDGE_CURVE('',#6767,#6767,#5680,.T.);
#8629=EDGE_CURVE('',#6767,#6768,#3881,.T.);
#8630=EDGE_CURVE('',#6768,#6768,#5681,.T.);
#8631=EDGE_CURVE('',#6768,#6769,#3882,.T.);
#8632=EDGE_CURVE('',#6769,#6769,#5682,.T.);
#8633=EDGE_CURVE('',#6770,#6771,#5683,.T.);
#8634=EDGE_CURVE('',#6772,#6772,#5684,.T.);
#8635=EDGE_CURVE('',#6772,#6773,#3883,.T.);
#8636=EDGE_CURVE('',#6773,#6773,#5685,.T.);
#8637=EDGE_CURVE('',#6774,#6774,#5686,.T.);
#8638=EDGE_CURVE('',#6774,#6775,#3884,.T.);
#8639=EDGE_CURVE('',#6775,#6775,#5687,.T.);
#8640=EDGE_CURVE('',#6776,#6777,#5688,.T.);
#8641=EDGE_CURVE('',#6778,#6777,#5689,.T.);
#8642=EDGE_CURVE('',#6776,#6778,#5690,.T.);
#8643=EDGE_CURVE('',#6778,#6779,#5691,.T.);
#8644=EDGE_CURVE('',#6779,#6780,#5692,.T.);
#8645=EDGE_CURVE('',#6776,#6780,#5693,.T.);
#8646=EDGE_CURVE('',#6778,#6781,#3885,.T.);
#8647=EDGE_CURVE('',#6781,#6782,#965,.T.);
#8648=EDGE_CURVE('',#6782,#6783,#5694,.T.);
#8649=EDGE_CURVE('',#6783,#6784,#966,.T.);
#8650=EDGE_CURVE('',#6784,#6779,#3886,.T.);
#8651=EDGE_CURVE('',#6785,#6786,#5695,.T.);
#8652=EDGE_CURVE('',#6786,#6783,#967,.T.);
#8653=EDGE_CURVE('',#6782,#6785,#968,.T.);
#8654=EDGE_CURVE('',#6787,#6786,#969,.T.);
#8655=EDGE_CURVE('',#6785,#6788,#970,.T.);
#8656=EDGE_CURVE('',#6789,#6788,#5696,.T.);
#8657=EDGE_CURVE('',#6788,#6790,#971,.T.);
#8658=EDGE_CURVE('',#6791,#6790,#5697,.T.);
#8659=EDGE_CURVE('',#6791,#6792,#5698,.T.);
#8660=EDGE_CURVE('',#6787,#6792,#5699,.T.);
#8661=EDGE_CURVE('',#6793,#6794,#972,.T.);
#8662=EDGE_CURVE('',#6794,#6795,#973,.T.);
#8663=EDGE_CURVE('',#6795,#6796,#5700,.T.);
#8664=EDGE_CURVE('',#6796,#6774,#3887,.T.);
#8665=EDGE_CURVE('',#6796,#6797,#5701,.T.);
#8666=EDGE_CURVE('',#6797,#6798,#67,.T.);
#8667=EDGE_CURVE('',#6798,#6793,#974,.T.);
#8668=EDGE_CURVE('',#6780,#6799,#5702,.T.);
#8669=EDGE_CURVE('',#6799,#6797,#975,.T.);
#8670=EDGE_CURVE('',#6795,#6800,#976,.T.);
#8671=EDGE_CURVE('',#6800,#6776,#5703,.T.);
#8672=EDGE_CURVE('',#6801,#6791,#3888,.T.);
#8673=EDGE_CURVE('',#6801,#6802,#977,.T.);
#8674=EDGE_CURVE('',#6802,#6803,#3889,.T.);
#8675=EDGE_CURVE('',#6803,#6803,#5704,.T.);
#8676=EDGE_CURVE('',#6802,#6804,#978,.T.);
#8677=EDGE_CURVE('',#6792,#6804,#3890,.T.);
#8678=EDGE_CURVE('',#6801,#6790,#5705,.T.);
#8679=EDGE_CURVE('',#6787,#6804,#5706,.T.);
#8680=EDGE_CURVE('',#6790,#6805,#979,.T.);
#8681=EDGE_CURVE('',#6805,#6806,#980,.T.);
#8682=EDGE_CURVE('',#6806,#6807,#981,.T.);
#8683=EDGE_CURVE('',#6808,#6807,#3891,.T.);
#8684=EDGE_CURVE('',#6808,#6809,#982,.T.);
#8685=EDGE_CURVE('',#6809,#6810,#983,.T.);
#8686=EDGE_CURVE('',#6810,#6811,#984,.T.);
#8687=EDGE_CURVE('',#6811,#6812,#3892,.T.);
#8688=EDGE_CURVE('',#6812,#6813,#985,.T.);
#8689=EDGE_CURVE('',#6813,#6814,#986,.T.);
#8690=EDGE_CURVE('',#6814,#6787,#987,.T.);
#8691=EDGE_CURVE('',#6807,#6815,#5707,.T.);
#8692=EDGE_CURVE('',#6816,#6815,#3893,.T.);
#8693=EDGE_CURVE('',#6816,#6808,#5708,.T.);
#8694=EDGE_CURVE('',#6811,#6817,#5709,.T.);
#8695=EDGE_CURVE('',#6817,#6818,#3894,.T.);
#8696=EDGE_CURVE('',#6818,#6812,#5710,.T.);
#8697=EDGE_CURVE('',#6817,#6819,#5711,.T.);
#8698=EDGE_CURVE('',#6819,#6818,#3895,.T.);
#8699=EDGE_CURVE('',#6815,#6777,#3896,.T.);
#8700=EDGE_CURVE('',#6777,#6816,#5712,.T.);
#8701=EDGE_CURVE('',#6786,#6814,#5713,.T.);
#8702=EDGE_CURVE('',#6783,#6813,#5714,.T.);
#8703=EDGE_CURVE('',#6784,#6812,#5715,.T.);
#8704=EDGE_CURVE('',#6784,#6818,#5716,.T.);
#8705=EDGE_CURVE('',#6779,#6819,#5717,.T.);
#8706=EDGE_CURVE('',#6780,#6819,#5718,.T.);
#8707=EDGE_CURVE('',#6799,#6817,#5719,.T.);
#8708=EDGE_CURVE('',#6799,#6811,#5720,.T.);
#8709=EDGE_CURVE('',#6798,#6810,#988,.T.);
#8710=EDGE_CURVE('',#6794,#6809,#989,.T.);
#8711=EDGE_CURVE('',#6800,#6808,#5721,.T.);
#8712=EDGE_CURVE('',#6800,#6816,#5722,.T.);
#8713=EDGE_CURVE('',#6781,#6815,#5723,.T.);
#8714=EDGE_CURVE('',#6781,#6807,#5724,.T.);
#8715=EDGE_CURVE('',#6782,#6806,#5725,.T.);
#8716=EDGE_CURVE('',#6785,#6805,#5726,.T.);
#8717=EDGE_CURVE('',#6820,#6821,#5727,.T.);
#8718=EDGE_CURVE('',#6820,#6822,#5728,.T.);
#8719=EDGE_CURVE('',#6822,#6823,#5729,.T.);
#8720=EDGE_CURVE('',#6823,#6821,#5730,.T.);
#8721=EDGE_CURVE('',#6824,#6824,#5731,.T.);
#8722=EDGE_CURVE('',#6824,#6825,#3897,.T.);
#8723=EDGE_CURVE('',#6825,#6825,#5732,.T.);
#8724=EDGE_CURVE('',#6821,#6823,#5733,.T.);
#8725=EDGE_CURVE('',#6823,#6822,#5734,.T.);
#8726=EDGE_CURVE('',#6822,#6820,#5735,.T.);
#8727=EDGE_CURVE('',#6822,#6826,#3898,.T.);
#8728=EDGE_CURVE('',#6826,#6826,#5736,.T.);
#8729=EDGE_CURVE('',#6826,#6827,#3899,.T.);
#8730=EDGE_CURVE('',#6827,#6827,#5737,.T.);
#8731=EDGE_CURVE('',#6827,#6828,#3900,.T.);
#8732=EDGE_CURVE('',#6828,#6828,#5738,.T.);
#8733=EDGE_CURVE('',#6829,#6830,#5739,.T.);
#8734=EDGE_CURVE('',#6831,#6829,#990,.T.);
#8735=EDGE_CURVE('',#6832,#6831,#991,.T.);
#8736=EDGE_CURVE('',#6833,#6832,#5740,.T.);
#8737=EDGE_CURVE('',#6834,#6833,#5741,.T.);
#8738=EDGE_CURVE('',#6835,#6834,#992,.T.);
#8739=EDGE_CURVE('',#6835,#6830,#993,.T.);
#8740=EDGE_CURVE('',#6836,#6837,#5742,.T.);
#8741=EDGE_CURVE('',#6837,#6838,#3901,.T.);
#8742=EDGE_CURVE('',#6838,#6839,#5743,.T.);
#8743=EDGE_CURVE('',#6840,#6839,#994,.T.);
#8744=EDGE_CURVE('',#6840,#6841,#5744,.T.);
#8745=EDGE_CURVE('',#6829,#6841,#3902,.T.);
#8746=EDGE_CURVE('',#6830,#6836,#995,.T.);
#8747=EDGE_CURVE('',#6842,#6842,#5745,.T.);
#8748=EDGE_CURVE('',#6842,#6843,#3903,.T.);
#8749=EDGE_CURVE('',#6843,#6843,#5746,.T.);
#8750=EDGE_CURVE('',#6844,#6845,#5747,.T.);
#8751=EDGE_CURVE('',#6845,#6846,#996,.T.);
#8752=EDGE_CURVE('',#6847,#6846,#5748,.T.);
#8753=EDGE_CURVE('',#6847,#6848,#997,.T.);
#8754=EDGE_CURVE('',#6848,#6849,#5749,.T.);
#8755=EDGE_CURVE('',#6849,#6844,#5750,.T.);
#8756=EDGE_CURVE('',#6849,#6841,#5751,.T.);
#8757=EDGE_CURVE('',#6840,#6839,#5752,.T.);
#8758=EDGE_CURVE('',#6838,#6844,#5753,.T.);
#8759=EDGE_CURVE('',#6839,#6850,#3904,.T.);
#8760=EDGE_CURVE('',#6850,#6850,#5754,.T.);
#8761=EDGE_CURVE('',#6834,#6851,#5755,.T.);
#8762=EDGE_CURVE('',#6851,#6842,#3905,.T.);
#8763=EDGE_CURVE('',#6851,#6852,#5756,.T.);
#8764=EDGE_CURVE('',#6852,#6853,#998,.T.);
#8765=EDGE_CURVE('',#6853,#6835,#999,.T.);
#8766=EDGE_CURVE('',#6846,#6854,#5757,.T.);
#8767=EDGE_CURVE('',#6854,#6855,#5758,.T.);
#8768=EDGE_CURVE('',#6856,#6855,#5759,.T.);
#8769=EDGE_CURVE('',#6855,#6852,#5760,.T.);
#8770=EDGE_CURVE('',#6833,#6857,#5761,.T.);
#8771=EDGE_CURVE('',#6832,#6847,#5762,.T.);
#8772=EDGE_CURVE('',#6841,#6858,#3906,.T.);
#8773=EDGE_CURVE('',#6858,#6859,#1000,.T.);
#8774=EDGE_CURVE('',#6859,#6831,#5763,.T.);
#8775=EDGE_CURVE('',#6837,#6860,#1001,.T.);
#8776=EDGE_CURVE('',#6860,#6861,#5764,.T.);
#8777=EDGE_CURVE('',#6861,#6862,#1002,.T.);
#8778=EDGE_CURVE('',#6862,#6838,#3907,.T.);
#8779=EDGE_CURVE('',#6862,#6845,#5765,.T.);
#8780=EDGE_CURVE('',#6848,#6858,#5766,.T.);
#8781=EDGE_CURVE('',#6846,#6861,#5767,.T.);
#8782=EDGE_CURVE('',#6854,#6860,#1003,.T.);
#8783=EDGE_CURVE('',#6853,#6836,#1004,.T.);
#8784=EDGE_CURVE('',#6847,#6859,#5768,.T.);
#8785=EDGE_CURVE('',#6863,#6864,#5769,.T.);
#8786=EDGE_CURVE('',#6863,#6865,#5770,.T.);
#8787=EDGE_CURVE('',#6865,#6866,#5771,.T.);
#8788=EDGE_CURVE('',#6866,#6864,#5772,.T.);
#8789=EDGE_CURVE('',#6867,#6867,#5773,.T.);
#8790=EDGE_CURVE('',#6867,#6868,#3908,.T.);
#8791=EDGE_CURVE('',#6868,#6868,#5774,.T.);
#8792=EDGE_CURVE('',#6864,#6866,#5775,.T.);
#8793=EDGE_CURVE('',#6866,#6865,#5776,.T.);
#8794=EDGE_CURVE('',#6865,#6863,#5777,.T.);
#8795=EDGE_CURVE('',#6865,#6869,#3909,.T.);
#8796=EDGE_CURVE('',#6869,#6869,#5778,.T.);
#8797=EDGE_CURVE('',#6869,#6870,#3910,.T.);
#8798=EDGE_CURVE('',#6870,#6870,#5779,.T.);
#8799=EDGE_CURVE('',#6870,#6871,#3911,.T.);
#8800=EDGE_CURVE('',#6871,#6871,#5780,.T.);
#8801=EDGE_CURVE('',#6872,#6873,#5781,.T.);
#8802=EDGE_CURVE('',#6873,#6872,#5782,.T.);
#8803=EDGE_CURVE('',#6873,#6874,#5783,.T.);
#8804=EDGE_CURVE('',#6874,#6874,#5784,.T.);
#8805=EDGE_CURVE('',#6875,#6875,#5785,.T.);
#8806=EDGE_CURVE('',#6875,#6876,#3912,.T.);
#8807=EDGE_CURVE('',#6876,#6876,#5786,.T.);
#8808=EDGE_CURVE('',#6877,#6878,#5787,.T.);
#8809=EDGE_CURVE('',#6878,#6877,#5788,.T.);
#8810=EDGE_CURVE('',#6878,#6875,#3913,.T.);
#8811=EDGE_CURVE('',#6877,#6879,#3914,.T.);
#8812=EDGE_CURVE('',#6880,#6879,#5789,.T.);
#8813=EDGE_CURVE('',#6879,#6880,#5790,.T.);
#8814=EDGE_CURVE('',#6881,#6881,#5791,.T.);
#8815=EDGE_CURVE('',#6881,#6880,#3915,.T.);
#8816=EDGE_CURVE('',#6882,#6882,#5792,.T.);
#8817=EDGE_CURVE('',#6882,#6883,#3916,.T.);
#8818=EDGE_CURVE('',#6883,#6883,#5793,.T.);
#8819=EDGE_CURVE('',#6872,#6884,#3917,.T.);
#8820=EDGE_CURVE('',#6884,#6884,#5794,.T.);
#8821=EDGE_CURVE('',#6885,#6886,#5795,.T.);
#8822=EDGE_CURVE('',#6887,#6885,#5796,.T.);
#8823=EDGE_CURVE('',#6888,#6887,#5797,.T.);
#8824=EDGE_CURVE('',#6886,#6888,#5798,.T.);
#8825=EDGE_CURVE('',#6889,#6890,#5799,.T.);
#8826=EDGE_CURVE('',#6891,#6889,#3918,.T.);
#8827=EDGE_CURVE('',#6891,#6892,#5800,.T.);
#8828=EDGE_CURVE('',#6890,#6892,#3919,.T.);
#8829=EDGE_CURVE('',#6892,#6893,#5801,.T.);
#8830=EDGE_CURVE('',#6894,#6892,#5802,.T.);
#8831=EDGE_CURVE('',#6895,#6894,#5803,.T.);
#8832=EDGE_CURVE('',#6893,#6895,#5804,.T.);
#8833=EDGE_CURVE('',#6896,#6897,#5805,.T.);
#8834=EDGE_CURVE('',#6896,#6898,#5806,.T.);
#8835=EDGE_CURVE('',#6899,#6898,#5807,.T.);
#8836=EDGE_CURVE('',#6899,#6897,#5808,.T.);
#8837=EDGE_CURVE('',#6900,#6901,#5809,.T.);
#8838=EDGE_CURVE('',#6902,#6901,#3920,.T.);
#8839=EDGE_CURVE('',#6902,#6903,#5810,.T.);
#8840=EDGE_CURVE('',#6900,#6903,#3921,.T.);
#8841=EDGE_CURVE('',#6903,#6904,#5811,.T.);
#8842=EDGE_CURVE('',#6905,#6903,#5812,.T.);
#8843=EDGE_CURVE('',#6906,#6905,#5813,.T.);
#8844=EDGE_CURVE('',#6906,#6904,#5814,.T.);
#8845=EDGE_CURVE('',#6907,#6908,#5815,.T.);
#8846=EDGE_CURVE('',#6909,#6908,#3922,.T.);
#8847=EDGE_CURVE('',#6909,#6910,#5816,.T.);
#8848=EDGE_CURVE('',#6907,#6910,#3923,.T.);
#8849=EDGE_CURVE('',#6910,#6911,#5817,.T.);
#8850=EDGE_CURVE('',#6912,#6910,#5818,.T.);
#8851=EDGE_CURVE('',#6913,#6912,#5819,.T.);
#8852=EDGE_CURVE('',#6913,#6911,#5820,.T.);
#8853=EDGE_CURVE('',#6914,#6915,#5821,.T.);
#8854=EDGE_CURVE('',#6914,#6916,#5822,.T.);
#8855=EDGE_CURVE('',#6917,#6916,#5823,.T.);
#8856=EDGE_CURVE('',#6915,#6917,#5824,.T.);
#8857=EDGE_CURVE('',#6918,#6919,#5825,.T.);
#8858=EDGE_CURVE('',#6920,#6918,#3924,.T.);
#8859=EDGE_CURVE('',#6914,#6920,#5826,.T.);
#8860=EDGE_CURVE('',#6919,#6914,#3925,.T.);
#8861=EDGE_CURVE('',#6911,#6921,#3926,.T.);
#8862=EDGE_CURVE('',#6921,#6907,#5827,.T.);
#8863=EDGE_CURVE('',#6904,#6922,#3927,.T.);
#8864=EDGE_CURVE('',#6922,#6900,#5828,.T.);
#8865=EDGE_CURVE('',#6897,#6923,#3928,.T.);
#8866=EDGE_CURVE('',#6923,#6924,#5829,.T.);
#8867=EDGE_CURVE('',#6924,#6896,#3929,.T.);
#8868=EDGE_CURVE('',#6925,#6925,#5830,.T.);
#8869=EDGE_CURVE('',#6925,#6926,#3930,.T.);
#8870=EDGE_CURVE('',#6926,#6926,#5831,.T.);
#8871=EDGE_CURVE('',#6927,#6927,#5832,.T.);
#8872=EDGE_CURVE('',#6927,#6928,#3931,.T.);
#8873=EDGE_CURVE('',#6928,#6928,#5833,.T.);
#8874=EDGE_CURVE('',#6929,#6930,#5834,.T.);
#8875=EDGE_CURVE('',#6930,#6931,#3932,.T.);
#8876=EDGE_CURVE('',#6931,#6932,#5835,.T.);
#8877=EDGE_CURVE('',#6932,#6929,#3933,.T.);
#8878=EDGE_CURVE('',#6889,#6933,#5836,.T.);
#8879=EDGE_CURVE('',#6933,#6934,#3934,.T.);
#8880=EDGE_CURVE('',#6934,#6891,#5837,.T.);
#8881=EDGE_CURVE('',#6908,#6920,#5838,.T.);
#8882=EDGE_CURVE('',#6918,#6909,#5839,.T.);
#8883=EDGE_CURVE('',#6901,#6935,#5840,.T.);
#8884=EDGE_CURVE('',#6935,#6936,#3935,.T.);
#8885=EDGE_CURVE('',#6936,#6902,#5841,.T.);
#8886=EDGE_CURVE('',#6937,#6938,#5842,.T.);
#8887=EDGE_CURVE('',#6938,#6939,#3936,.T.);
#8888=EDGE_CURVE('',#6939,#6940,#5843,.T.);
#8889=EDGE_CURVE('',#6940,#6937,#3937,.T.);
#8890=EDGE_CURVE('',#6941,#6942,#5844,.T.);
#8891=EDGE_CURVE('',#6941,#6933,#5845,.T.);
#8892=EDGE_CURVE('',#6889,#6942,#5846,.T.);
#8893=EDGE_CURVE('',#6943,#6944,#5847,.T.);
#8894=EDGE_CURVE('',#6943,#6930,#5848,.T.);
#8895=EDGE_CURVE('',#6929,#6944,#5849,.T.);
#8896=EDGE_CURVE('',#6918,#6945,#5850,.T.);
#8897=EDGE_CURVE('',#6912,#6945,#5851,.T.);
#8898=EDGE_CURVE('',#6912,#6909,#5852,.T.);
#8899=EDGE_CURVE('',#6936,#6913,#5853,.T.);
#8900=EDGE_CURVE('',#6905,#6913,#5854,.T.);
#8901=EDGE_CURVE('',#6905,#6902,#5855,.T.);
#8902=EDGE_CURVE('',#6946,#6947,#5856,.T.);
#8903=EDGE_CURVE('',#6946,#6899,#5857,.T.);
#8904=EDGE_CURVE('',#6948,#6899,#5858,.T.);
#8905=EDGE_CURVE('',#6948,#6947,#5859,.T.);
#8906=EDGE_CURVE('',#6934,#6917,#5860,.T.);
#8907=EDGE_CURVE('',#6894,#6917,#5861,.T.);
#8908=EDGE_CURVE('',#6894,#6891,#5862,.T.);
#8909=EDGE_CURVE('',#6931,#6895,#5863,.T.);
#8910=EDGE_CURVE('',#6887,#6895,#5864,.T.);
#8911=EDGE_CURVE('',#6887,#6932,#5865,.T.);
#8912=EDGE_CURVE('',#6916,#6949,#5866,.T.);
#8913=EDGE_CURVE('',#6916,#6920,#5867,.T.);
#8914=EDGE_CURVE('',#6908,#6949,#5868,.T.);
#8915=EDGE_CURVE('',#6950,#6951,#5869,.T.);
#8916=EDGE_CURVE('',#6950,#6935,#5870,.T.);
#8917=EDGE_CURVE('',#6901,#6951,#5871,.T.);
#8918=EDGE_CURVE('',#6952,#6888,#5872,.T.);
#8919=EDGE_CURVE('',#6952,#6953,#5873,.T.);
#8920=EDGE_CURVE('',#6954,#6953,#5874,.T.);
#8921=EDGE_CURVE('',#6954,#6888,#5875,.T.);
#8922=EDGE_CURVE('',#6945,#6941,#5876,.T.);
#8923=EDGE_CURVE('',#6942,#6943,#5877,.T.);
#8924=EDGE_CURVE('',#6944,#6948,#5878,.T.);
#8925=EDGE_CURVE('',#6898,#6906,#5879,.T.);
#8926=EDGE_CURVE('',#6953,#6946,#3938,.T.);
#8927=EDGE_CURVE('',#6947,#6954,#3939,.T.);
#8928=EDGE_CURVE('',#6949,#6950,#5880,.T.);
#8929=EDGE_CURVE('',#6951,#6955,#5881,.T.);
#8930=EDGE_CURVE('',#6955,#6956,#5882,.T.);
#8931=EDGE_CURVE('',#6956,#6952,#5883,.T.);
#8932=EDGE_CURVE('',#6939,#6906,#5884,.T.);
#8933=EDGE_CURVE('',#6898,#6940,#5885,.T.);
#8934=EDGE_CURVE('',#6955,#6938,#5886,.T.);
#8935=EDGE_CURVE('',#6937,#6956,#5887,.T.);
#8936=EDGE_CURVE('',#6886,#6957,#3940,.T.);
#8937=EDGE_CURVE('',#6957,#6958,#5888,.T.);
#8938=EDGE_CURVE('',#6958,#6885,#3941,.T.);
#8939=EDGE_CURVE('',#6915,#6959,#3942,.T.);
#8940=EDGE_CURVE('',#6959,#6919,#5889,.T.);
#8941=EDGE_CURVE('',#6893,#6960,#3943,.T.);
#8942=EDGE_CURVE('',#6960,#6890,#5890,.T.);
#8943=EDGE_CURVE('',#6945,#6919,#5891,.T.);
#8944=EDGE_CURVE('',#6941,#6959,#5892,.T.);
#8945=EDGE_CURVE('',#6933,#6959,#5893,.T.);
#8946=EDGE_CURVE('',#6915,#6934,#5894,.T.);
#8947=EDGE_CURVE('',#6936,#6911,#5895,.T.);
#8948=EDGE_CURVE('',#6921,#6935,#5896,.T.);
#8949=EDGE_CURVE('',#6921,#6950,#5897,.T.);
#8950=EDGE_CURVE('',#6907,#6949,#5898,.T.);
#8951=EDGE_CURVE('',#6939,#6904,#5899,.T.);
#8952=EDGE_CURVE('',#6922,#6938,#5900,.T.);
#8953=EDGE_CURVE('',#6922,#6955,#5901,.T.);
#8954=EDGE_CURVE('',#6900,#6951,#5902,.T.);
#8955=EDGE_CURVE('',#6952,#6923,#5903,.T.);
#8956=EDGE_CURVE('',#6924,#6956,#5904,.T.);
#8957=EDGE_CURVE('',#6953,#6923,#5905,.T.);
#8958=EDGE_CURVE('',#6924,#6937,#5906,.T.);
#8959=EDGE_CURVE('',#6946,#6897,#5907,.T.);
#8960=EDGE_CURVE('',#6896,#6940,#5908,.T.);
#8961=EDGE_CURVE('',#6893,#6931,#5909,.T.);
#8962=EDGE_CURVE('',#6960,#6930,#5910,.T.);
#8963=EDGE_CURVE('',#6942,#6890,#5911,.T.);
#8964=EDGE_CURVE('',#6960,#6943,#5912,.T.);
#8965=EDGE_CURVE('',#6932,#6885,#5913,.T.);
#8966=EDGE_CURVE('',#6886,#6954,#5914,.T.);
#8967=EDGE_CURVE('',#6929,#6958,#5915,.T.);
#8968=EDGE_CURVE('',#6957,#6947,#5916,.T.);
#8969=EDGE_CURVE('',#6944,#6958,#5917,.T.);
#8970=EDGE_CURVE('',#6957,#6948,#5918,.T.);
#8971=EDGE_CURVE('',#6961,#6961,#5919,.T.);
#8972=EDGE_CURVE('',#6961,#6962,#3944,.T.);
#8973=EDGE_CURVE('',#6962,#6962,#5920,.T.);
#8974=EDGE_CURVE('',#6963,#6964,#5921,.T.);
#8975=EDGE_CURVE('',#6964,#6963,#5922,.T.);
#8976=EDGE_CURVE('',#6964,#6965,#3945,.T.);
#8977=EDGE_CURVE('',#6965,#6965,#5923,.T.);
#8978=EDGE_CURVE('',#6966,#6967,#5924,.T.);
#8979=EDGE_CURVE('',#6967,#6966,#5925,.T.);
#8980=EDGE_CURVE('',#6967,#6968,#3946,.T.);
#8981=EDGE_CURVE('',#6968,#6968,#5926,.T.);
#8982=EDGE_CURVE('',#6969,#6969,#5927,.T.);
#8983=EDGE_CURVE('',#6969,#6970,#3947,.T.);
#8984=EDGE_CURVE('',#6970,#6970,#5928,.T.);
#8985=EDGE_CURVE('',#6971,#6972,#5929,.T.);
#8986=EDGE_CURVE('',#6973,#6971,#238,.T.);
#8987=EDGE_CURVE('',#6974,#6973,#5930,.T.);
#8988=EDGE_CURVE('',#6972,#6974,#239,.T.);
#8989=EDGE_CURVE('',#6975,#6976,#5931,.T.);
#8990=EDGE_CURVE('',#6976,#6975,#5932,.T.);
#8991=EDGE_CURVE('',#6976,#6977,#3948,.T.);
#8992=EDGE_CURVE('',#6977,#6977,#5933,.T.);
#8993=EDGE_CURVE('',#6978,#6979,#5934,.T.);
#8994=EDGE_CURVE('',#6979,#6978,#5935,.T.);
#8995=EDGE_CURVE('',#6979,#6980,#3949,.T.);
#8996=EDGE_CURVE('',#6980,#6980,#5936,.T.);
#8997=EDGE_CURVE('',#6981,#6981,#5937,.T.);
#8998=EDGE_CURVE('',#6981,#6982,#3950,.T.);
#8999=EDGE_CURVE('',#6982,#6982,#5938,.T.);
#9000=EDGE_CURVE('',#6983,#6983,#5939,.T.);
#9001=EDGE_CURVE('',#6983,#6984,#3951,.T.);
#9002=EDGE_CURVE('',#6984,#6984,#5940,.T.);
#9003=EDGE_CURVE('',#6985,#6986,#5941,.T.);
#9004=EDGE_CURVE('',#6987,#6985,#240,.T.);
#9005=EDGE_CURVE('',#6988,#6987,#5942,.T.);
#9006=EDGE_CURVE('',#6986,#6988,#241,.T.);
#9007=EDGE_CURVE('',#6978,#6989,#3952,.T.);
#9008=EDGE_CURVE('',#6990,#6989,#5943,.T.);
#9009=EDGE_CURVE('',#6991,#6990,#1005,.F.);
#9010=EDGE_CURVE('',#6989,#6991,#5944,.T.);
#9011=EDGE_CURVE('',#6992,#6992,#5945,.T.);
#9012=EDGE_CURVE('',#6992,#6961,#3953,.T.);
#9013=EDGE_CURVE('',#6975,#6969,#3954,.T.);
#9014=EDGE_CURVE('',#6972,#6985,#3955,.T.);
#9015=EDGE_CURVE('',#6991,#6986,#3956,.T.);
#9016=EDGE_CURVE('',#6971,#6990,#3957,.T.);
#9017=EDGE_CURVE('',#6966,#6981,#3958,.T.);
#9018=EDGE_CURVE('',#6963,#6983,#3959,.T.);
#9019=EDGE_CURVE('',#6993,#6994,#3960,.T.);
#9020=EDGE_CURVE('',#6993,#6995,#3961,.T.);
#9021=EDGE_CURVE('',#6995,#6996,#3962,.T.);
#9022=EDGE_CURVE('',#6994,#6996,#3963,.T.);
#9023=EDGE_CURVE('',#6997,#6998,#3964,.T.);
#9024=EDGE_CURVE('',#6998,#6999,#3965,.T.);
#9025=EDGE_CURVE('',#6999,#7000,#3966,.T.);
#9026=EDGE_CURVE('',#7000,#6997,#3967,.T.);
#9027=EDGE_CURVE('',#7001,#6987,#3968,.T.);
#9028=EDGE_CURVE('',#7001,#7002,#5946,.T.);
#9029=EDGE_CURVE('',#7003,#7002,#3969,.T.);
#9030=EDGE_CURVE('',#7004,#7003,#3970,.T.);
#9031=EDGE_CURVE('',#6996,#7004,#3971,.T.);
#9032=EDGE_CURVE('',#6995,#7005,#3972,.T.);
#9033=EDGE_CURVE('',#7005,#7006,#3973,.T.);
#9034=EDGE_CURVE('',#7006,#7007,#3974,.T.);
#9035=EDGE_CURVE('',#7008,#7007,#3975,.T.);
#9036=EDGE_CURVE('',#7009,#7008,#3976,.T.);
#9037=EDGE_CURVE('',#7010,#7009,#3977,.T.);
#9038=EDGE_CURVE('',#7011,#7010,#3978,.T.);
#9039=EDGE_CURVE('',#7011,#7012,#5947,.T.);
#9040=EDGE_CURVE('',#6988,#7012,#3979,.T.);
#9041=EDGE_CURVE('',#7007,#7013,#3980,.T.);
#9042=EDGE_CURVE('',#7014,#7013,#3981,.T.);
#9043=EDGE_CURVE('',#7014,#7008,#3982,.T.);
#9044=EDGE_CURVE('',#7015,#6974,#3983,.T.);
#9045=EDGE_CURVE('',#6973,#7016,#3984,.T.);
#9046=EDGE_CURVE('',#7016,#7017,#5948,.T.);
#9047=EDGE_CURVE('',#7017,#7018,#3985,.T.);
#9048=EDGE_CURVE('',#7018,#7019,#3986,.T.);
#9049=EDGE_CURVE('',#7019,#7014,#3987,.T.);
#9050=EDGE_CURVE('',#7013,#7020,#3988,.T.);
#9051=EDGE_CURVE('',#7020,#7021,#3989,.T.);
#9052=EDGE_CURVE('',#7021,#7022,#3990,.T.);
#9053=EDGE_CURVE('',#7022,#7023,#3991,.T.);
#9054=EDGE_CURVE('',#7023,#7024,#3992,.T.);
#9055=EDGE_CURVE('',#7024,#7025,#3993,.T.);
#9056=EDGE_CURVE('',#7025,#6993,#3994,.T.);
#9057=EDGE_CURVE('',#6994,#7026,#3995,.T.);
#9058=EDGE_CURVE('',#7026,#7027,#3996,.T.);
#9059=EDGE_CURVE('',#7027,#7028,#3997,.T.);
#9060=EDGE_CURVE('',#7028,#7015,#5949,.T.);
#9061=EDGE_CURVE('',#7029,#7030,#3998,.T.);
#9062=EDGE_CURVE('',#7030,#7031,#3999,.T.);
#9063=EDGE_CURVE('',#7031,#7032,#4000,.T.);
#9064=EDGE_CURVE('',#7029,#7032,#4001,.T.);
#9065=EDGE_CURVE('',#7033,#7034,#4002,.T.);
#9066=EDGE_CURVE('',#7034,#7035,#4003,.T.);
#9067=EDGE_CURVE('',#7035,#7036,#4004,.T.);
#9068=EDGE_CURVE('',#7036,#7037,#4005,.T.);
#9069=EDGE_CURVE('',#7038,#7037,#4006,.T.);
#9070=EDGE_CURVE('',#7029,#7038,#4007,.T.);
#9071=EDGE_CURVE('',#7032,#7033,#4008,.T.);
#9072=EDGE_CURVE('',#7039,#7040,#4009,.T.);
#9073=EDGE_CURVE('',#7040,#7041,#4010,.T.);
#9074=EDGE_CURVE('',#7041,#7042,#4011,.T.);
#9075=EDGE_CURVE('',#7042,#7043,#4012,.T.);
#9076=EDGE_CURVE('',#7043,#7044,#5950,.T.);
#9077=EDGE_CURVE('',#7044,#7045,#4013,.T.);
#9078=EDGE_CURVE('',#7045,#7039,#4014,.T.);
#9079=EDGE_CURVE('',#7046,#7047,#4015,.T.);
#9080=EDGE_CURVE('',#7047,#7048,#4016,.T.);
#9081=EDGE_CURVE('',#7048,#7049,#4017,.T.);
#9082=EDGE_CURVE('',#7049,#7050,#4018,.T.);
#9083=EDGE_CURVE('',#7050,#7051,#5951,.T.);
#9084=EDGE_CURVE('',#7051,#7052,#4019,.T.);
#9085=EDGE_CURVE('',#7052,#7053,#4020,.T.);
#9086=EDGE_CURVE('',#7053,#7054,#4021,.T.);
#9087=EDGE_CURVE('',#7054,#7046,#4022,.T.);
#9088=EDGE_CURVE('',#7055,#7056,#4023,.T.);
#9089=EDGE_CURVE('',#7056,#7057,#5952,.T.);
#9090=EDGE_CURVE('',#7058,#7057,#4024,.T.);
#9091=EDGE_CURVE('',#7058,#7055,#5953,.T.);
#9092=EDGE_CURVE('',#7012,#7056,#1006,.T.);
#9093=EDGE_CURVE('',#7055,#7016,#1007,.T.);
#9094=EDGE_CURVE('',#7059,#7060,#4025,.T.);
#9095=EDGE_CURVE('',#7060,#7001,#1008,.T.);
#9096=EDGE_CURVE('',#7015,#7059,#1009,.T.);
#9097=EDGE_CURVE('',#7061,#7062,#4026,.T.);
#9098=EDGE_CURVE('',#7062,#7060,#5954,.T.);
#9099=EDGE_CURVE('',#7059,#7061,#5955,.T.);
#9100=EDGE_CURVE('',#7002,#7062,#1010,.T.);
#9101=EDGE_CURVE('',#7061,#7028,#1011,.T.);
#9102=EDGE_CURVE('',#7027,#7003,#4027,.T.);
#9103=EDGE_CURVE('',#7026,#7004,#4028,.T.);
#9104=EDGE_CURVE('',#7019,#7009,#4029,.T.);
#9105=EDGE_CURVE('',#7018,#7010,#4030,.T.);
#9106=EDGE_CURVE('',#7057,#7011,#1012,.T.);
#9107=EDGE_CURVE('',#7017,#7058,#1013,.T.);
#9108=EDGE_CURVE('',#7031,#7063,#4031,.T.);
#9109=EDGE_CURVE('',#7063,#7064,#4032,.T.);
#9110=EDGE_CURVE('',#7064,#7065,#5956,.T.);
#9111=EDGE_CURVE('',#7065,#7066,#4033,.T.);
#9112=EDGE_CURVE('',#7066,#7033,#4034,.T.);
#9113=EDGE_CURVE('',#7066,#7067,#4035,.T.);
#9114=EDGE_CURVE('',#7067,#7034,#4036,.T.);
#9115=EDGE_CURVE('',#7063,#7068,#4037,.T.);
#9116=EDGE_CURVE('',#7068,#7069,#4038,.T.);
#9117=EDGE_CURVE('',#7064,#7069,#4039,.T.);
#9118=EDGE_CURVE('',#7065,#7070,#4040,.T.);
#9119=EDGE_CURVE('',#7070,#7067,#4041,.T.);
#9120=EDGE_CURVE('',#7069,#7070,#5957,.T.);
#9121=EDGE_CURVE('',#7071,#7072,#4042,.T.);
#9122=EDGE_CURVE('',#7072,#7030,#4043,.T.);
#9123=EDGE_CURVE('',#7038,#7071,#5958,.T.);
#9124=EDGE_CURVE('',#7073,#7074,#4044,.T.);
#9125=EDGE_CURVE('',#7074,#7072,#4045,.T.);
#9126=EDGE_CURVE('',#7071,#7073,#4046,.T.);
#9127=EDGE_CURVE('',#7037,#7073,#5959,.T.);
#9128=EDGE_CURVE('',#7025,#7042,#5960,.T.);
#9129=EDGE_CURVE('',#6993,#7041,#68,.T.);
#9130=EDGE_CURVE('',#6995,#7040,#69,.T.);
#9131=EDGE_CURVE('',#7042,#7074,#5961,.T.);
#9132=EDGE_CURVE('',#7043,#7073,#5962,.T.);
#9133=EDGE_CURVE('',#7005,#7039,#5963,.T.);
#9134=EDGE_CURVE('',#7052,#7020,#5964,.T.);
#9135=EDGE_CURVE('',#7053,#7013,#70,.T.);
#9136=EDGE_CURVE('',#7044,#7037,#5965,.T.);
#9137=EDGE_CURVE('',#7005,#6997,#5966,.T.);
#9138=EDGE_CURVE('',#6997,#7039,#5967,.T.);
#9139=EDGE_CURVE('',#7054,#7007,#71,.T.);
#9140=EDGE_CURVE('',#7068,#7052,#5968,.T.);
#9141=EDGE_CURVE('',#7069,#7051,#5969,.T.);
#9142=EDGE_CURVE('',#7045,#7036,#5970,.T.);
#9143=EDGE_CURVE('',#6998,#7045,#5971,.T.);
#9144=EDGE_CURVE('',#7006,#7000,#5972,.T.);
#9145=EDGE_CURVE('',#7046,#7006,#5973,.T.);
#9146=EDGE_CURVE('',#7070,#7050,#5974,.T.);
#9147=EDGE_CURVE('',#6998,#7036,#5975,.T.);
#9148=EDGE_CURVE('',#7046,#7000,#5976,.T.);
#9149=EDGE_CURVE('',#7067,#7049,#72,.T.);
#9150=EDGE_CURVE('',#6999,#7035,#5977,.T.);
#9151=EDGE_CURVE('',#7047,#6999,#5978,.T.);
#9152=EDGE_CURVE('',#7034,#7048,#73,.T.);
#9153=EDGE_CURVE('',#7047,#7035,#5979,.T.);
#9154=EDGE_CURVE('',#7074,#7025,#5980,.T.);
#9155=EDGE_CURVE('',#7072,#7024,#74,.T.);
#9156=EDGE_CURVE('',#7030,#7023,#75,.T.);
#9157=EDGE_CURVE('',#7031,#7022,#76,.T.);
#9158=EDGE_CURVE('',#7063,#7021,#77,.T.);
#9159=EDGE_CURVE('',#7068,#7020,#5981,.T.);
#9160=EDGE_CURVE('',#7075,#7075,#5982,.T.);
#9161=EDGE_CURVE('',#7075,#7076,#5983,.T.);
#9162=EDGE_CURVE('',#7077,#7076,#5984,.T.);
#9163=EDGE_CURVE('',#7076,#7077,#5985,.T.);
#9164=EDGE_CURVE('',#7078,#7079,#5986,.T.);
#9165=EDGE_CURVE('',#7079,#7078,#5987,.T.);
#9166=EDGE_CURVE('',#7079,#7080,#5988,.T.);
#9167=EDGE_CURVE('',#7080,#7080,#5989,.T.);
#9168=EDGE_CURVE('',#7078,#7077,#4047,.T.);
#9169=EDGE_CURVE('',#7081,#7081,#5990,.T.);
#9170=EDGE_CURVE('',#7081,#7082,#4048,.T.);
#9171=EDGE_CURVE('',#7082,#7082,#5991,.T.);
#9172=EDGE_CURVE('',#7083,#7084,#5992,.T.);
#9173=EDGE_CURVE('',#7084,#7085,#5993,.T.);
#9174=EDGE_CURVE('',#7085,#7086,#4049,.T.);
#9175=EDGE_CURVE('',#7086,#7086,#5994,.T.);
#9176=EDGE_CURVE('',#7085,#7083,#5995,.T.);
#9177=EDGE_CURVE('',#7087,#7087,#5996,.T.);
#9178=EDGE_CURVE('',#7087,#7088,#4050,.T.);
#9179=EDGE_CURVE('',#7088,#7088,#5997,.T.);
#9180=EDGE_CURVE('',#7089,#7089,#5998,.T.);
#9181=EDGE_CURVE('',#7089,#7090,#4051,.T.);
#9182=EDGE_CURVE('',#7090,#7090,#5999,.T.);
#9183=EDGE_CURVE('',#7091,#7091,#6000,.T.);
#9184=EDGE_CURVE('',#7091,#7092,#4052,.T.);
#9185=EDGE_CURVE('',#7092,#7092,#6001,.T.);
#9186=EDGE_CURVE('',#7093,#7093,#6002,.T.);
#9187=EDGE_CURVE('',#7093,#7094,#4053,.T.);
#9188=EDGE_CURVE('',#7094,#7094,#6003,.T.);
#9189=EDGE_CURVE('',#7095,#7083,#4054,.T.);
#9190=EDGE_CURVE('',#7096,#7095,#4055,.T.);
#9191=EDGE_CURVE('',#7096,#7084,#4056,.T.);
#9192=EDGE_CURVE('',#7097,#7098,#4057,.T.);
#9193=EDGE_CURVE('',#7098,#7099,#6004,.T.);
#9194=EDGE_CURVE('',#7100,#7099,#4058,.T.);
#9195=EDGE_CURVE('',#7097,#7100,#6005,.T.);
#9196=EDGE_CURVE('',#7099,#7101,#4059,.T.);
#9197=EDGE_CURVE('',#7102,#7101,#4060,.T.);
#9198=EDGE_CURVE('',#7100,#7102,#4061,.T.);
#9199=EDGE_CURVE('',#7095,#7097,#4062,.T.);
#9200=EDGE_CURVE('',#7102,#7096,#4063,.T.);
#9201=EDGE_CURVE('',#7103,#7104,#4064,.T.);
#9202=EDGE_CURVE('',#7105,#7103,#4065,.T.);
#9203=EDGE_CURVE('',#7106,#7105,#4066,.T.);
#9204=EDGE_CURVE('',#7107,#7106,#6006,.T.);
#9205=EDGE_CURVE('',#7104,#7107,#4067,.T.);
#9206=EDGE_CURVE('',#7084,#7103,#4068,.T.);
#9207=EDGE_CURVE('',#7083,#7104,#4069,.T.);
#9208=EDGE_CURVE('',#7108,#7109,#4070,.T.);
#9209=EDGE_CURVE('',#7098,#7108,#4071,.T.);
#9210=EDGE_CURVE('',#7110,#7107,#4072,.T.);
#9211=EDGE_CURVE('',#7109,#7110,#4073,.T.);
#9212=EDGE_CURVE('',#7111,#7106,#4074,.T.);
#9213=EDGE_CURVE('',#7111,#7110,#6007,.T.);
#9214=EDGE_CURVE('',#7112,#7105,#4075,.T.);
#9215=EDGE_CURVE('',#7112,#7111,#4076,.T.);
#9216=EDGE_CURVE('',#7101,#7113,#4077,.T.);
#9217=EDGE_CURVE('',#7113,#7114,#4078,.T.);
#9218=EDGE_CURVE('',#7114,#7112,#4079,.T.);
#9219=EDGE_CURVE('',#7113,#7108,#4080,.T.);
#9220=EDGE_CURVE('',#7114,#7109,#4081,.T.);
#9221=EDGE_CURVE('',#7115,#7115,#6008,.T.);
#9222=EDGE_CURVE('',#7115,#7116,#4082,.T.);
#9223=EDGE_CURVE('',#7116,#7116,#6009,.T.);
#9224=EDGE_CURVE('',#7117,#7118,#6010,.T.);
#9225=EDGE_CURVE('',#7119,#7119,#6011,.T.);
#9226=EDGE_CURVE('',#7119,#7120,#6012,.T.);
#9227=EDGE_CURVE('',#7120,#7120,#6013,.T.);
#9228=EDGE_CURVE('',#7121,#7122,#6014,.T.);
#9229=EDGE_CURVE('',#7122,#7121,#6015,.T.);
#9230=EDGE_CURVE('',#7122,#7123,#4083,.T.);
#9231=EDGE_CURVE('',#7123,#7123,#6016,.T.);
#9232=EDGE_CURVE('',#7124,#7125,#6017,.T.);
#9233=EDGE_CURVE('',#7125,#7124,#6018,.T.);
#9234=EDGE_CURVE('',#7125,#7126,#4084,.T.);
#9235=EDGE_CURVE('',#7126,#7127,#6019,.T.);
#9236=EDGE_CURVE('',#7127,#7126,#6020,.T.);
#9237=EDGE_CURVE('',#7121,#7127,#4085,.T.);
#9238=EDGE_CURVE('',#7128,#7129,#6021,.T.);
#9239=EDGE_CURVE('',#7129,#7128,#6022,.T.);
#9240=EDGE_CURVE('',#7129,#7124,#4086,.T.);
#9241=EDGE_CURVE('',#7130,#7131,#6023,.T.);
#9242=EDGE_CURVE('',#7131,#7130,#6024,.T.);
#9243=EDGE_CURVE('',#7131,#7132,#4087,.T.);
#9244=EDGE_CURVE('',#7132,#7133,#6025,.T.);
#9245=EDGE_CURVE('',#7133,#7132,#6026,.T.);
#9246=EDGE_CURVE('',#7128,#7133,#4088,.T.);
#9247=EDGE_CURVE('',#7134,#7135,#6027,.T.);
#9248=EDGE_CURVE('',#7135,#7134,#6028,.T.);
#9249=EDGE_CURVE('',#7135,#7130,#4089,.T.);
#9250=EDGE_CURVE('',#7136,#7137,#6029,.T.);
#9251=EDGE_CURVE('',#7137,#7136,#6030,.T.);
#9252=EDGE_CURVE('',#7137,#7138,#4090,.T.);
#9253=EDGE_CURVE('',#7138,#7139,#6031,.T.);
#9254=EDGE_CURVE('',#7139,#7138,#6032,.T.);
#9255=EDGE_CURVE('',#7134,#7139,#4091,.T.);
#9256=EDGE_CURVE('',#7140,#7141,#6033,.T.);
#9257=EDGE_CURVE('',#7141,#7140,#6034,.T.);
#9258=EDGE_CURVE('',#7141,#7136,#4092,.T.);
#9259=EDGE_CURVE('',#7142,#7143,#6035,.T.);
#9260=EDGE_CURVE('',#7143,#7142,#6036,.T.);
#9261=EDGE_CURVE('',#7143,#7144,#4093,.T.);
#9262=EDGE_CURVE('',#7144,#7145,#6037,.T.);
#9263=EDGE_CURVE('',#7145,#7144,#6038,.T.);
#9264=EDGE_CURVE('',#7140,#7145,#4094,.T.);
#9265=EDGE_CURVE('',#7146,#7147,#6039,.T.);
#9266=EDGE_CURVE('',#7147,#7146,#6040,.T.);
#9267=EDGE_CURVE('',#7147,#7142,#4095,.T.);
#9268=EDGE_CURVE('',#7148,#7149,#6041,.T.);
#9269=EDGE_CURVE('',#7149,#7148,#6042,.T.);
#9270=EDGE_CURVE('',#7149,#7150,#4096,.T.);
#9271=EDGE_CURVE('',#7150,#7151,#6043,.T.);
#9272=EDGE_CURVE('',#7151,#7150,#6044,.T.);
#9273=EDGE_CURVE('',#7146,#7151,#4097,.T.);
#9274=EDGE_CURVE('',#7152,#7153,#6045,.T.);
#9275=EDGE_CURVE('',#7153,#7152,#6046,.T.);
#9276=EDGE_CURVE('',#7153,#7148,#4098,.T.);
#9277=EDGE_CURVE('',#7154,#7155,#6047,.T.);
#9278=EDGE_CURVE('',#7155,#7154,#6048,.T.);
#9279=EDGE_CURVE('',#7155,#7156,#4099,.T.);
#9280=EDGE_CURVE('',#7156,#7157,#6049,.T.);
#9281=EDGE_CURVE('',#7157,#7156,#6050,.T.);
#9282=EDGE_CURVE('',#7152,#7157,#4100,.T.);
#9283=EDGE_CURVE('',#7158,#7159,#6051,.T.);
#9284=EDGE_CURVE('',#7159,#7158,#6052,.T.);
#9285=EDGE_CURVE('',#7159,#7154,#4101,.T.);
#9286=EDGE_CURVE('',#7160,#7161,#6053,.T.);
#9287=EDGE_CURVE('',#7161,#7160,#6054,.T.);
#9288=EDGE_CURVE('',#7161,#7162,#4102,.T.);
#9289=EDGE_CURVE('',#7162,#7163,#6055,.T.);
#9290=EDGE_CURVE('',#7163,#7162,#6056,.T.);
#9291=EDGE_CURVE('',#7158,#7163,#4103,.T.);
#9292=EDGE_CURVE('',#7164,#7165,#6057,.T.);
#9293=EDGE_CURVE('',#7165,#7164,#6058,.T.);
#9294=EDGE_CURVE('',#7165,#7160,#4104,.T.);
#9295=EDGE_CURVE('',#7166,#7167,#6059,.T.);
#9296=EDGE_CURVE('',#7167,#7166,#6060,.T.);
#9297=EDGE_CURVE('',#7167,#7168,#4105,.T.);
#9298=EDGE_CURVE('',#7168,#7169,#6061,.T.);
#9299=EDGE_CURVE('',#7169,#7168,#6062,.T.);
#9300=EDGE_CURVE('',#7164,#7169,#4106,.T.);
#9301=EDGE_CURVE('',#7170,#7171,#6063,.T.);
#9302=EDGE_CURVE('',#7171,#7170,#6064,.T.);
#9303=EDGE_CURVE('',#7171,#7166,#4107,.T.);
#9304=EDGE_CURVE('',#7172,#7173,#6065,.T.);
#9305=EDGE_CURVE('',#7173,#7172,#6066,.T.);
#9306=EDGE_CURVE('',#7173,#7174,#4108,.T.);
#9307=EDGE_CURVE('',#7174,#7175,#6067,.T.);
#9308=EDGE_CURVE('',#7175,#7174,#6068,.T.);
#9309=EDGE_CURVE('',#7170,#7175,#4109,.T.);
#9310=EDGE_CURVE('',#7176,#7177,#6069,.T.);
#9311=EDGE_CURVE('',#7177,#7176,#6070,.T.);
#9312=EDGE_CURVE('',#7177,#7172,#4110,.T.);
#9313=EDGE_CURVE('',#7178,#7179,#6071,.T.);
#9314=EDGE_CURVE('',#7179,#7178,#6072,.T.);
#9315=EDGE_CURVE('',#7179,#7180,#4111,.T.);
#9316=EDGE_CURVE('',#7180,#7181,#6073,.T.);
#9317=EDGE_CURVE('',#7181,#7180,#6074,.T.);
#9318=EDGE_CURVE('',#7176,#7181,#4112,.T.);
#9319=EDGE_CURVE('',#7182,#7183,#6075,.T.);
#9320=EDGE_CURVE('',#7183,#7182,#6076,.T.);
#9321=EDGE_CURVE('',#7183,#7178,#4113,.T.);
#9322=EDGE_CURVE('',#7184,#7185,#6077,.T.);
#9323=EDGE_CURVE('',#7185,#7184,#6078,.T.);
#9324=EDGE_CURVE('',#7185,#7186,#4114,.T.);
#9325=EDGE_CURVE('',#7186,#7187,#6079,.T.);
#9326=EDGE_CURVE('',#7187,#7186,#6080,.T.);
#9327=EDGE_CURVE('',#7182,#7187,#4115,.T.);
#9328=EDGE_CURVE('',#7188,#7189,#6081,.T.);
#9329=EDGE_CURVE('',#7189,#7188,#6082,.T.);
#9330=EDGE_CURVE('',#7189,#7184,#4116,.T.);
#9331=EDGE_CURVE('',#7190,#7191,#6083,.T.);
#9332=EDGE_CURVE('',#7191,#7190,#6084,.T.);
#9333=EDGE_CURVE('',#7191,#7192,#4117,.T.);
#9334=EDGE_CURVE('',#7192,#7193,#6085,.T.);
#9335=EDGE_CURVE('',#7193,#7192,#6086,.T.);
#9336=EDGE_CURVE('',#7188,#7193,#4118,.T.);
#9337=EDGE_CURVE('',#7194,#7195,#6087,.T.);
#9338=EDGE_CURVE('',#7195,#7194,#6088,.T.);
#9339=EDGE_CURVE('',#7195,#7190,#4119,.T.);
#9340=EDGE_CURVE('',#7196,#7197,#6089,.T.);
#9341=EDGE_CURVE('',#7197,#7196,#6090,.T.);
#9342=EDGE_CURVE('',#7197,#7198,#4120,.T.);
#9343=EDGE_CURVE('',#7198,#7199,#6091,.T.);
#9344=EDGE_CURVE('',#7199,#7198,#6092,.T.);
#9345=EDGE_CURVE('',#7194,#7199,#4121,.T.);
#9346=EDGE_CURVE('',#7200,#7201,#6093,.T.);
#9347=EDGE_CURVE('',#7201,#7200,#6094,.T.);
#9348=EDGE_CURVE('',#7201,#7196,#4122,.T.);
#9349=EDGE_CURVE('',#7202,#7203,#6095,.T.);
#9350=EDGE_CURVE('',#7203,#7202,#6096,.T.);
#9351=EDGE_CURVE('',#7203,#7204,#4123,.T.);
#9352=EDGE_CURVE('',#7204,#7205,#6097,.T.);
#9353=EDGE_CURVE('',#7205,#7204,#6098,.T.);
#9354=EDGE_CURVE('',#7200,#7205,#4124,.T.);
#9355=EDGE_CURVE('',#7206,#7207,#6099,.T.);
#9356=EDGE_CURVE('',#7207,#7206,#6100,.T.);
#9357=EDGE_CURVE('',#7207,#7202,#4125,.T.);
#9358=EDGE_CURVE('',#7208,#7209,#6101,.T.);
#9359=EDGE_CURVE('',#7209,#7208,#6102,.T.);
#9360=EDGE_CURVE('',#7209,#7210,#4126,.T.);
#9361=EDGE_CURVE('',#7210,#7211,#6103,.T.);
#9362=EDGE_CURVE('',#7211,#7210,#6104,.T.);
#9363=EDGE_CURVE('',#7206,#7211,#4127,.T.);
#9364=EDGE_CURVE('',#7212,#7213,#242,.T.);
#9365=EDGE_CURVE('',#7212,#7214,#6105,.T.);
#9366=EDGE_CURVE('',#7215,#7214,#243,.T.);
#9367=EDGE_CURVE('',#7216,#7215,#244,.T.);
#9368=EDGE_CURVE('',#7216,#7217,#6106,.T.);
#9369=EDGE_CURVE('',#7218,#7217,#245,.T.);
#9370=EDGE_CURVE('',#7219,#7218,#246,.T.);
#9371=EDGE_CURVE('',#7219,#7220,#6107,.T.);
#9372=EDGE_CURVE('',#7221,#7220,#247,.T.);
#9373=EDGE_CURVE('',#7222,#7221,#248,.T.);
#9374=EDGE_CURVE('',#7222,#7223,#6108,.T.);
#9375=EDGE_CURVE('',#7224,#7223,#249,.T.);
#9376=EDGE_CURVE('',#7225,#7224,#250,.T.);
#9377=EDGE_CURVE('',#7225,#7226,#6109,.T.);
#9378=EDGE_CURVE('',#7227,#7226,#251,.T.);
#9379=EDGE_CURVE('',#7228,#7227,#252,.T.);
#9380=EDGE_CURVE('',#7228,#7229,#6110,.T.);
#9381=EDGE_CURVE('',#7230,#7229,#253,.T.);
#9382=EDGE_CURVE('',#7231,#7230,#254,.T.);
#9383=EDGE_CURVE('',#7231,#7232,#6111,.T.);
#9384=EDGE_CURVE('',#7233,#7232,#255,.T.);
#9385=EDGE_CURVE('',#7234,#7233,#256,.T.);
#9386=EDGE_CURVE('',#7234,#7235,#6112,.T.);
#9387=EDGE_CURVE('',#7236,#7235,#257,.T.);
#9388=EDGE_CURVE('',#7237,#7236,#258,.T.);
#9389=EDGE_CURVE('',#7237,#7238,#6113,.T.);
#9390=EDGE_CURVE('',#7239,#7238,#259,.T.);
#9391=EDGE_CURVE('',#7240,#7239,#260,.T.);
#9392=EDGE_CURVE('',#7240,#7241,#6114,.T.);
#9393=EDGE_CURVE('',#7242,#7241,#261,.T.);
#9394=EDGE_CURVE('',#7243,#7242,#262,.T.);
#9395=EDGE_CURVE('',#7243,#7244,#6115,.T.);
#9396=EDGE_CURVE('',#7245,#7244,#263,.T.);
#9397=EDGE_CURVE('',#7246,#7245,#264,.T.);
#9398=EDGE_CURVE('',#7246,#7247,#6116,.T.);
#9399=EDGE_CURVE('',#7248,#7247,#265,.T.);
#9400=EDGE_CURVE('',#7249,#7248,#266,.T.);
#9401=EDGE_CURVE('',#7249,#7250,#6117,.T.);
#9402=EDGE_CURVE('',#7251,#7250,#267,.T.);
#9403=EDGE_CURVE('',#7252,#7251,#268,.T.);
#9404=EDGE_CURVE('',#7252,#7253,#6118,.T.);
#9405=EDGE_CURVE('',#7254,#7253,#269,.T.);
#9406=EDGE_CURVE('',#7255,#7254,#270,.T.);
#9407=EDGE_CURVE('',#7255,#7256,#6119,.T.);
#9408=EDGE_CURVE('',#7257,#7256,#271,.T.);
#9409=EDGE_CURVE('',#7258,#7257,#272,.T.);
#9410=EDGE_CURVE('',#7258,#7259,#6120,.T.);
#9411=EDGE_CURVE('',#7260,#7259,#273,.T.);
#9412=EDGE_CURVE('',#7261,#7260,#274,.T.);
#9413=EDGE_CURVE('',#7261,#7262,#6121,.T.);
#9414=EDGE_CURVE('',#7263,#7262,#275,.T.);
#9415=EDGE_CURVE('',#7264,#7263,#276,.T.);
#9416=EDGE_CURVE('',#7264,#7265,#6122,.T.);
#9417=EDGE_CURVE('',#7266,#7265,#277,.T.);
#9418=EDGE_CURVE('',#7267,#7266,#278,.T.);
#9419=EDGE_CURVE('',#7267,#7268,#6123,.T.);
#9420=EDGE_CURVE('',#7269,#7268,#279,.T.);
#9421=EDGE_CURVE('',#7270,#7269,#280,.T.);
#9422=EDGE_CURVE('',#7270,#7271,#6124,.T.);
#9423=EDGE_CURVE('',#7272,#7271,#281,.T.);
#9424=EDGE_CURVE('',#7273,#7272,#282,.T.);
#9425=EDGE_CURVE('',#7273,#7274,#6125,.T.);
#9426=EDGE_CURVE('',#7275,#7274,#283,.T.);
#9427=EDGE_CURVE('',#7276,#7275,#284,.T.);
#9428=EDGE_CURVE('',#7276,#7277,#6126,.T.);
#9429=EDGE_CURVE('',#7278,#7277,#285,.T.);
#9430=EDGE_CURVE('',#7279,#7278,#286,.T.);
#9431=EDGE_CURVE('',#7279,#7280,#6127,.T.);
#9432=EDGE_CURVE('',#7281,#7280,#287,.T.);
#9433=EDGE_CURVE('',#7282,#7281,#288,.T.);
#9434=EDGE_CURVE('',#7282,#7283,#6128,.T.);
#9435=EDGE_CURVE('',#7284,#7283,#289,.T.);
#9436=EDGE_CURVE('',#7285,#7284,#290,.T.);
#9437=EDGE_CURVE('',#7285,#7286,#6129,.T.);
#9438=EDGE_CURVE('',#7287,#7286,#291,.T.);
#9439=EDGE_CURVE('',#7288,#7287,#292,.T.);
#9440=EDGE_CURVE('',#7288,#7289,#6130,.T.);
#9441=EDGE_CURVE('',#7290,#7289,#293,.T.);
#9442=EDGE_CURVE('',#7291,#7290,#294,.T.);
#9443=EDGE_CURVE('',#7291,#7292,#6131,.T.);
#9444=EDGE_CURVE('',#7293,#7292,#295,.T.);
#9445=EDGE_CURVE('',#7294,#7293,#296,.T.);
#9446=EDGE_CURVE('',#7294,#7295,#6132,.T.);
#9447=EDGE_CURVE('',#7296,#7295,#297,.T.);
#9448=EDGE_CURVE('',#7297,#7296,#298,.T.);
#9449=EDGE_CURVE('',#7297,#7298,#6133,.T.);
#9450=EDGE_CURVE('',#7299,#7298,#299,.T.);
#9451=EDGE_CURVE('',#7300,#7299,#300,.T.);
#9452=EDGE_CURVE('',#7300,#7301,#6134,.T.);
#9453=EDGE_CURVE('',#7302,#7301,#301,.T.);
#9454=EDGE_CURVE('',#7303,#7302,#302,.T.);
#9455=EDGE_CURVE('',#7303,#7304,#6135,.T.);
#9456=EDGE_CURVE('',#7305,#7304,#303,.T.);
#9457=EDGE_CURVE('',#7306,#7305,#304,.T.);
#9458=EDGE_CURVE('',#7306,#7307,#6136,.T.);
#9459=EDGE_CURVE('',#7308,#7307,#305,.T.);
#9460=EDGE_CURVE('',#7309,#7308,#306,.T.);
#9461=EDGE_CURVE('',#7309,#7310,#6137,.T.);
#9462=EDGE_CURVE('',#7311,#7310,#307,.T.);
#9463=EDGE_CURVE('',#7312,#7311,#308,.T.);
#9464=EDGE_CURVE('',#7312,#7313,#6138,.T.);
#9465=EDGE_CURVE('',#7314,#7313,#309,.T.);
#9466=EDGE_CURVE('',#7315,#7314,#310,.T.);
#9467=EDGE_CURVE('',#7315,#7316,#6139,.T.);
#9468=EDGE_CURVE('',#7317,#7316,#311,.T.);
#9469=EDGE_CURVE('',#7318,#7317,#312,.T.);
#9470=EDGE_CURVE('',#7318,#7319,#6140,.T.);
#9471=EDGE_CURVE('',#7320,#7319,#313,.T.);
#9472=EDGE_CURVE('',#7321,#7320,#314,.T.);
#9473=EDGE_CURVE('',#7321,#7322,#6141,.T.);
#9474=EDGE_CURVE('',#7323,#7322,#315,.T.);
#9475=EDGE_CURVE('',#7324,#7323,#316,.T.);
#9476=EDGE_CURVE('',#7324,#7325,#6142,.T.);
#9477=EDGE_CURVE('',#7326,#7325,#317,.T.);
#9478=EDGE_CURVE('',#7327,#7326,#318,.T.);
#9479=EDGE_CURVE('',#7327,#7328,#6143,.T.);
#9480=EDGE_CURVE('',#7329,#7328,#319,.F.);
#9481=EDGE_CURVE('',#7329,#7330,#4128,.T.);
#9482=EDGE_CURVE('',#7330,#7330,#6144,.T.);
#9483=EDGE_CURVE('',#7331,#7329,#320,.F.);
#9484=EDGE_CURVE('',#7332,#7331,#321,.T.);
#9485=EDGE_CURVE('',#7332,#7333,#6145,.T.);
#9486=EDGE_CURVE('',#7334,#7333,#322,.T.);
#9487=EDGE_CURVE('',#7335,#7334,#323,.T.);
#9488=EDGE_CURVE('',#7335,#7336,#6146,.T.);
#9489=EDGE_CURVE('',#7337,#7336,#324,.T.);
#9490=EDGE_CURVE('',#7338,#7337,#325,.T.);
#9491=EDGE_CURVE('',#7338,#7339,#6147,.T.);
#9492=EDGE_CURVE('',#7340,#7339,#326,.T.);
#9493=EDGE_CURVE('',#7341,#7340,#327,.T.);
#9494=EDGE_CURVE('',#7341,#7342,#6148,.T.);
#9495=EDGE_CURVE('',#7343,#7342,#328,.T.);
#9496=EDGE_CURVE('',#7344,#7343,#329,.T.);
#9497=EDGE_CURVE('',#7344,#7345,#6149,.T.);
#9498=EDGE_CURVE('',#7346,#7345,#330,.T.);
#9499=EDGE_CURVE('',#7347,#7346,#331,.T.);
#9500=EDGE_CURVE('',#7347,#7348,#6150,.T.);
#9501=EDGE_CURVE('',#7349,#7348,#332,.T.);
#9502=EDGE_CURVE('',#7350,#7349,#333,.T.);
#9503=EDGE_CURVE('',#7350,#7351,#6151,.T.);
#9504=EDGE_CURVE('',#7352,#7351,#334,.T.);
#9505=EDGE_CURVE('',#7353,#7352,#335,.T.);
#9506=EDGE_CURVE('',#7353,#7354,#6152,.T.);
#9507=EDGE_CURVE('',#7355,#7354,#336,.T.);
#9508=EDGE_CURVE('',#7356,#7355,#337,.T.);
#9509=EDGE_CURVE('',#7356,#7357,#6153,.T.);
#9510=EDGE_CURVE('',#7358,#7357,#338,.T.);
#9511=EDGE_CURVE('',#7359,#7358,#339,.T.);
#9512=EDGE_CURVE('',#7359,#7360,#6154,.T.);
#9513=EDGE_CURVE('',#7361,#7360,#340,.T.);
#9514=EDGE_CURVE('',#7362,#7361,#341,.T.);
#9515=EDGE_CURVE('',#7362,#7363,#6155,.T.);
#9516=EDGE_CURVE('',#7364,#7363,#342,.T.);
#9517=EDGE_CURVE('',#7365,#7364,#343,.T.);
#9518=EDGE_CURVE('',#7365,#7366,#6156,.T.);
#9519=EDGE_CURVE('',#7367,#7366,#344,.T.);
#9520=EDGE_CURVE('',#7368,#7367,#345,.T.);
#9521=EDGE_CURVE('',#7368,#7369,#6157,.T.);
#9522=EDGE_CURVE('',#7370,#7369,#346,.T.);
#9523=EDGE_CURVE('',#7371,#7370,#347,.T.);
#9524=EDGE_CURVE('',#7371,#7372,#6158,.T.);
#9525=EDGE_CURVE('',#7373,#7372,#348,.T.);
#9526=EDGE_CURVE('',#7374,#7373,#349,.T.);
#9527=EDGE_CURVE('',#7374,#7375,#6159,.T.);
#9528=EDGE_CURVE('',#7376,#7375,#350,.T.);
#9529=EDGE_CURVE('',#7377,#7376,#351,.T.);
#9530=EDGE_CURVE('',#7377,#7378,#6160,.T.);
#9531=EDGE_CURVE('',#7379,#7378,#352,.T.);
#9532=EDGE_CURVE('',#7380,#7379,#353,.T.);
#9533=EDGE_CURVE('',#7380,#7381,#6161,.T.);
#9534=EDGE_CURVE('',#7382,#7381,#354,.T.);
#9535=EDGE_CURVE('',#7383,#7382,#355,.T.);
#9536=EDGE_CURVE('',#7383,#7384,#6162,.T.);
#9537=EDGE_CURVE('',#7385,#7384,#356,.T.);
#9538=EDGE_CURVE('',#7386,#7385,#357,.T.);
#9539=EDGE_CURVE('',#7386,#7387,#6163,.T.);
#9540=EDGE_CURVE('',#7388,#7387,#358,.T.);
#9541=EDGE_CURVE('',#7389,#7388,#359,.T.);
#9542=EDGE_CURVE('',#7389,#7390,#6164,.T.);
#9543=EDGE_CURVE('',#7391,#7390,#360,.T.);
#9544=EDGE_CURVE('',#7392,#7391,#361,.T.);
#9545=EDGE_CURVE('',#7392,#7393,#6165,.T.);
#9546=EDGE_CURVE('',#7394,#7393,#362,.T.);
#9547=EDGE_CURVE('',#7395,#7394,#363,.T.);
#9548=EDGE_CURVE('',#7395,#7396,#6166,.T.);
#9549=EDGE_CURVE('',#7397,#7396,#364,.T.);
#9550=EDGE_CURVE('',#7398,#7397,#365,.T.);
#9551=EDGE_CURVE('',#7398,#7399,#6167,.T.);
#9552=EDGE_CURVE('',#7400,#7399,#366,.T.);
#9553=EDGE_CURVE('',#7401,#7400,#367,.T.);
#9554=EDGE_CURVE('',#7401,#7402,#6168,.T.);
#9555=EDGE_CURVE('',#7403,#7402,#368,.T.);
#9556=EDGE_CURVE('',#7404,#7403,#369,.T.);
#9557=EDGE_CURVE('',#7404,#7405,#6169,.T.);
#9558=EDGE_CURVE('',#7406,#7405,#370,.T.);
#9559=EDGE_CURVE('',#7407,#7406,#371,.T.);
#9560=EDGE_CURVE('',#7407,#7408,#6170,.T.);
#9561=EDGE_CURVE('',#7409,#7408,#372,.T.);
#9562=EDGE_CURVE('',#7410,#7409,#373,.T.);
#9563=EDGE_CURVE('',#7410,#7411,#6171,.T.);
#9564=EDGE_CURVE('',#7412,#7411,#374,.T.);
#9565=EDGE_CURVE('',#7413,#7412,#375,.T.);
#9566=EDGE_CURVE('',#7413,#7414,#6172,.T.);
#9567=EDGE_CURVE('',#7415,#7414,#376,.T.);
#9568=EDGE_CURVE('',#7416,#7415,#377,.T.);
#9569=EDGE_CURVE('',#7416,#7417,#6173,.T.);
#9570=EDGE_CURVE('',#7418,#7417,#378,.T.);
#9571=EDGE_CURVE('',#7419,#7418,#379,.T.);
#9572=EDGE_CURVE('',#7419,#7420,#6174,.T.);
#9573=EDGE_CURVE('',#7421,#7420,#380,.T.);
#9574=EDGE_CURVE('',#7422,#7421,#381,.T.);
#9575=EDGE_CURVE('',#7422,#7423,#6175,.T.);
#9576=EDGE_CURVE('',#7424,#7423,#382,.T.);
#9577=EDGE_CURVE('',#7425,#7424,#383,.T.);
#9578=EDGE_CURVE('',#7425,#7426,#6176,.T.);
#9579=EDGE_CURVE('',#7427,#7426,#384,.T.);
#9580=EDGE_CURVE('',#7428,#7427,#385,.T.);
#9581=EDGE_CURVE('',#7428,#7429,#6177,.T.);
#9582=EDGE_CURVE('',#7430,#7429,#386,.T.);
#9583=EDGE_CURVE('',#7431,#7430,#387,.T.);
#9584=EDGE_CURVE('',#7431,#7432,#6178,.T.);
#9585=EDGE_CURVE('',#7433,#7432,#388,.T.);
#9586=EDGE_CURVE('',#7434,#7433,#389,.T.);
#9587=EDGE_CURVE('',#7434,#7435,#6179,.T.);
#9588=EDGE_CURVE('',#7436,#7435,#390,.T.);
#9589=EDGE_CURVE('',#7437,#7436,#391,.T.);
#9590=EDGE_CURVE('',#7437,#7438,#6180,.T.);
#9591=EDGE_CURVE('',#7439,#7438,#392,.T.);
#9592=EDGE_CURVE('',#7440,#7439,#393,.T.);
#9593=EDGE_CURVE('',#7440,#7441,#6181,.T.);
#9594=EDGE_CURVE('',#7442,#7441,#394,.T.);
#9595=EDGE_CURVE('',#7443,#7442,#395,.T.);
#9596=EDGE_CURVE('',#7443,#7444,#6182,.T.);
#9597=EDGE_CURVE('',#7213,#7444,#396,.T.);
#9598=EDGE_CURVE('',#7445,#7446,#397,.F.);
#9599=EDGE_CURVE('',#7447,#7446,#6183,.T.);
#9600=EDGE_CURVE('',#7447,#7448,#398,.T.);
#9601=EDGE_CURVE('',#7448,#7449,#399,.T.);
#9602=EDGE_CURVE('',#7450,#7449,#6184,.T.);
#9603=EDGE_CURVE('',#7450,#7451,#400,.T.);
#9604=EDGE_CURVE('',#7451,#7452,#401,.T.);
#9605=EDGE_CURVE('',#7453,#7452,#6185,.T.);
#9606=EDGE_CURVE('',#7453,#7454,#402,.T.);
#9607=EDGE_CURVE('',#7454,#7455,#403,.T.);
#9608=EDGE_CURVE('',#7456,#7455,#6186,.T.);
#9609=EDGE_CURVE('',#7456,#7457,#404,.T.);
#9610=EDGE_CURVE('',#7457,#7458,#405,.T.);
#9611=EDGE_CURVE('',#7459,#7458,#6187,.T.);
#9612=EDGE_CURVE('',#7459,#7460,#406,.T.);
#9613=EDGE_CURVE('',#7460,#7461,#407,.T.);
#9614=EDGE_CURVE('',#7462,#7461,#6188,.T.);
#9615=EDGE_CURVE('',#7462,#7463,#408,.T.);
#9616=EDGE_CURVE('',#7463,#7464,#409,.T.);
#9617=EDGE_CURVE('',#7465,#7464,#6189,.T.);
#9618=EDGE_CURVE('',#7465,#7466,#410,.T.);
#9619=EDGE_CURVE('',#7466,#7467,#411,.T.);
#9620=EDGE_CURVE('',#7468,#7467,#6190,.T.);
#9621=EDGE_CURVE('',#7468,#7469,#412,.T.);
#9622=EDGE_CURVE('',#7469,#7470,#413,.T.);
#9623=EDGE_CURVE('',#7471,#7470,#6191,.T.);
#9624=EDGE_CURVE('',#7471,#7472,#414,.T.);
#9625=EDGE_CURVE('',#7472,#7473,#415,.T.);
#9626=EDGE_CURVE('',#7474,#7473,#6192,.T.);
#9627=EDGE_CURVE('',#7474,#7475,#416,.T.);
#9628=EDGE_CURVE('',#7475,#7476,#417,.T.);
#9629=EDGE_CURVE('',#7477,#7476,#6193,.T.);
#9630=EDGE_CURVE('',#7477,#7478,#418,.T.);
#9631=EDGE_CURVE('',#7478,#7479,#419,.T.);
#9632=EDGE_CURVE('',#7480,#7479,#6194,.T.);
#9633=EDGE_CURVE('',#7480,#7481,#420,.T.);
#9634=EDGE_CURVE('',#7481,#7482,#421,.T.);
#9635=EDGE_CURVE('',#7483,#7482,#6195,.T.);
#9636=EDGE_CURVE('',#7483,#7484,#422,.T.);
#9637=EDGE_CURVE('',#7484,#7485,#423,.T.);
#9638=EDGE_CURVE('',#7486,#7485,#6196,.T.);
#9639=EDGE_CURVE('',#7486,#7487,#424,.T.);
#9640=EDGE_CURVE('',#7487,#7488,#425,.T.);
#9641=EDGE_CURVE('',#7489,#7488,#6197,.T.);
#9642=EDGE_CURVE('',#7489,#7490,#426,.T.);
#9643=EDGE_CURVE('',#7490,#7491,#427,.T.);
#9644=EDGE_CURVE('',#7492,#7491,#6198,.T.);
#9645=EDGE_CURVE('',#7492,#7493,#428,.T.);
#9646=EDGE_CURVE('',#7493,#7494,#429,.T.);
#9647=EDGE_CURVE('',#7495,#7494,#6199,.T.);
#9648=EDGE_CURVE('',#7495,#7496,#430,.T.);
#9649=EDGE_CURVE('',#7496,#7497,#431,.T.);
#9650=EDGE_CURVE('',#7498,#7497,#6200,.T.);
#9651=EDGE_CURVE('',#7498,#7499,#432,.T.);
#9652=EDGE_CURVE('',#7499,#7500,#433,.T.);
#9653=EDGE_CURVE('',#7501,#7500,#6201,.T.);
#9654=EDGE_CURVE('',#7501,#7502,#434,.T.);
#9655=EDGE_CURVE('',#7502,#7503,#435,.T.);
#9656=EDGE_CURVE('',#7504,#7503,#6202,.T.);
#9657=EDGE_CURVE('',#7504,#7505,#436,.T.);
#9658=EDGE_CURVE('',#7505,#7506,#437,.T.);
#9659=EDGE_CURVE('',#7507,#7506,#6203,.T.);
#9660=EDGE_CURVE('',#7507,#7508,#438,.T.);
#9661=EDGE_CURVE('',#7508,#7509,#439,.T.);
#9662=EDGE_CURVE('',#7510,#7509,#6204,.T.);
#9663=EDGE_CURVE('',#7510,#7511,#440,.T.);
#9664=EDGE_CURVE('',#7511,#7512,#441,.T.);
#9665=EDGE_CURVE('',#7513,#7512,#6205,.T.);
#9666=EDGE_CURVE('',#7513,#7514,#442,.T.);
#9667=EDGE_CURVE('',#7514,#7515,#443,.T.);
#9668=EDGE_CURVE('',#7516,#7515,#6206,.T.);
#9669=EDGE_CURVE('',#7516,#7517,#444,.T.);
#9670=EDGE_CURVE('',#7517,#7518,#445,.T.);
#9671=EDGE_CURVE('',#7519,#7518,#6207,.T.);
#9672=EDGE_CURVE('',#7519,#7520,#446,.T.);
#9673=EDGE_CURVE('',#7520,#7521,#447,.T.);
#9674=EDGE_CURVE('',#7522,#7521,#6208,.T.);
#9675=EDGE_CURVE('',#7522,#7523,#448,.T.);
#9676=EDGE_CURVE('',#7523,#7524,#449,.T.);
#9677=EDGE_CURVE('',#7525,#7524,#6209,.T.);
#9678=EDGE_CURVE('',#7525,#7526,#450,.T.);
#9679=EDGE_CURVE('',#7526,#7527,#451,.T.);
#9680=EDGE_CURVE('',#7528,#7527,#6210,.T.);
#9681=EDGE_CURVE('',#7528,#7529,#452,.T.);
#9682=EDGE_CURVE('',#7529,#7530,#453,.T.);
#9683=EDGE_CURVE('',#7531,#7530,#6211,.T.);
#9684=EDGE_CURVE('',#7531,#7532,#454,.T.);
#9685=EDGE_CURVE('',#7532,#7533,#455,.T.);
#9686=EDGE_CURVE('',#7534,#7533,#6212,.T.);
#9687=EDGE_CURVE('',#7534,#7535,#456,.T.);
#9688=EDGE_CURVE('',#7535,#7536,#457,.T.);
#9689=EDGE_CURVE('',#7537,#7536,#6213,.T.);
#9690=EDGE_CURVE('',#7537,#7538,#458,.T.);
#9691=EDGE_CURVE('',#7538,#7539,#459,.T.);
#9692=EDGE_CURVE('',#7540,#7539,#6214,.T.);
#9693=EDGE_CURVE('',#7540,#7541,#460,.T.);
#9694=EDGE_CURVE('',#7541,#7542,#461,.T.);
#9695=EDGE_CURVE('',#7543,#7542,#6215,.T.);
#9696=EDGE_CURVE('',#7543,#7544,#462,.T.);
#9697=EDGE_CURVE('',#7544,#7545,#463,.T.);
#9698=EDGE_CURVE('',#7546,#7545,#6216,.T.);
#9699=EDGE_CURVE('',#7546,#7547,#464,.T.);
#9700=EDGE_CURVE('',#7547,#7548,#465,.T.);
#9701=EDGE_CURVE('',#7549,#7548,#6217,.T.);
#9702=EDGE_CURVE('',#7549,#7550,#466,.T.);
#9703=EDGE_CURVE('',#7550,#7551,#467,.T.);
#9704=EDGE_CURVE('',#7552,#7551,#6218,.T.);
#9705=EDGE_CURVE('',#7552,#7553,#468,.T.);
#9706=EDGE_CURVE('',#7553,#7554,#469,.T.);
#9707=EDGE_CURVE('',#7555,#7554,#6219,.T.);
#9708=EDGE_CURVE('',#7555,#7556,#470,.T.);
#9709=EDGE_CURVE('',#7556,#7557,#471,.T.);
#9710=EDGE_CURVE('',#7558,#7557,#6220,.T.);
#9711=EDGE_CURVE('',#7558,#7559,#472,.T.);
#9712=EDGE_CURVE('',#7559,#7560,#473,.T.);
#9713=EDGE_CURVE('',#7561,#7560,#6221,.T.);
#9714=EDGE_CURVE('',#7561,#7562,#474,.T.);
#9715=EDGE_CURVE('',#7562,#7563,#4129,.T.);
#9716=EDGE_CURVE('',#7563,#7563,#6222,.T.);
#9717=EDGE_CURVE('',#7562,#7564,#475,.T.);
#9718=EDGE_CURVE('',#7564,#7565,#476,.T.);
#9719=EDGE_CURVE('',#7566,#7565,#6223,.T.);
#9720=EDGE_CURVE('',#7566,#7567,#477,.T.);
#9721=EDGE_CURVE('',#7567,#7568,#478,.T.);
#9722=EDGE_CURVE('',#7569,#7568,#6224,.T.);
#9723=EDGE_CURVE('',#7569,#7570,#479,.T.);
#9724=EDGE_CURVE('',#7570,#7571,#480,.T.);
#9725=EDGE_CURVE('',#7572,#7571,#6225,.T.);
#9726=EDGE_CURVE('',#7572,#7573,#481,.T.);
#9727=EDGE_CURVE('',#7573,#7574,#482,.T.);
#9728=EDGE_CURVE('',#7575,#7574,#6226,.T.);
#9729=EDGE_CURVE('',#7575,#7576,#483,.T.);
#9730=EDGE_CURVE('',#7576,#7577,#484,.T.);
#9731=EDGE_CURVE('',#7578,#7577,#6227,.T.);
#9732=EDGE_CURVE('',#7578,#7579,#485,.T.);
#9733=EDGE_CURVE('',#7579,#7580,#486,.T.);
#9734=EDGE_CURVE('',#7581,#7580,#6228,.T.);
#9735=EDGE_CURVE('',#7581,#7582,#487,.T.);
#9736=EDGE_CURVE('',#7582,#7583,#488,.T.);
#9737=EDGE_CURVE('',#7584,#7583,#6229,.T.);
#9738=EDGE_CURVE('',#7584,#7585,#489,.T.);
#9739=EDGE_CURVE('',#7585,#7586,#490,.T.);
#9740=EDGE_CURVE('',#7587,#7586,#6230,.T.);
#9741=EDGE_CURVE('',#7587,#7588,#491,.T.);
#9742=EDGE_CURVE('',#7588,#7589,#492,.T.);
#9743=EDGE_CURVE('',#7590,#7589,#6231,.T.);
#9744=EDGE_CURVE('',#7590,#7591,#493,.T.);
#9745=EDGE_CURVE('',#7591,#7592,#494,.T.);
#9746=EDGE_CURVE('',#7593,#7592,#6232,.T.);
#9747=EDGE_CURVE('',#7593,#7594,#495,.T.);
#9748=EDGE_CURVE('',#7594,#7595,#496,.T.);
#9749=EDGE_CURVE('',#7596,#7595,#6233,.T.);
#9750=EDGE_CURVE('',#7596,#7597,#497,.T.);
#9751=EDGE_CURVE('',#7597,#7598,#498,.T.);
#9752=EDGE_CURVE('',#7599,#7598,#6234,.T.);
#9753=EDGE_CURVE('',#7599,#7600,#499,.T.);
#9754=EDGE_CURVE('',#7600,#7601,#500,.T.);
#9755=EDGE_CURVE('',#7602,#7601,#6235,.T.);
#9756=EDGE_CURVE('',#7602,#7603,#501,.T.);
#9757=EDGE_CURVE('',#7603,#7604,#502,.T.);
#9758=EDGE_CURVE('',#7605,#7604,#6236,.T.);
#9759=EDGE_CURVE('',#7605,#7606,#503,.T.);
#9760=EDGE_CURVE('',#7606,#7607,#504,.T.);
#9761=EDGE_CURVE('',#7608,#7607,#6237,.T.);
#9762=EDGE_CURVE('',#7608,#7609,#505,.T.);
#9763=EDGE_CURVE('',#7609,#7610,#506,.T.);
#9764=EDGE_CURVE('',#7611,#7610,#6238,.T.);
#9765=EDGE_CURVE('',#7611,#7612,#507,.T.);
#9766=EDGE_CURVE('',#7612,#7613,#508,.T.);
#9767=EDGE_CURVE('',#7614,#7613,#6239,.T.);
#9768=EDGE_CURVE('',#7614,#7615,#509,.T.);
#9769=EDGE_CURVE('',#7615,#7616,#510,.T.);
#9770=EDGE_CURVE('',#7617,#7616,#6240,.T.);
#9771=EDGE_CURVE('',#7617,#7618,#511,.T.);
#9772=EDGE_CURVE('',#7618,#7619,#512,.T.);
#9773=EDGE_CURVE('',#7620,#7619,#6241,.T.);
#9774=EDGE_CURVE('',#7620,#7621,#513,.T.);
#9775=EDGE_CURVE('',#7621,#7622,#514,.T.);
#9776=EDGE_CURVE('',#7623,#7622,#6242,.T.);
#9777=EDGE_CURVE('',#7623,#7624,#515,.T.);
#9778=EDGE_CURVE('',#7624,#7625,#516,.T.);
#9779=EDGE_CURVE('',#7626,#7625,#6243,.T.);
#9780=EDGE_CURVE('',#7626,#7627,#517,.T.);
#9781=EDGE_CURVE('',#7627,#7628,#518,.T.);
#9782=EDGE_CURVE('',#7629,#7628,#6244,.T.);
#9783=EDGE_CURVE('',#7629,#7630,#519,.T.);
#9784=EDGE_CURVE('',#7630,#7631,#520,.T.);
#9785=EDGE_CURVE('',#7632,#7631,#6245,.T.);
#9786=EDGE_CURVE('',#7632,#7633,#521,.T.);
#9787=EDGE_CURVE('',#7633,#7634,#522,.T.);
#9788=EDGE_CURVE('',#7635,#7634,#6246,.T.);
#9789=EDGE_CURVE('',#7635,#7636,#523,.T.);
#9790=EDGE_CURVE('',#7636,#7637,#524,.T.);
#9791=EDGE_CURVE('',#7638,#7637,#6247,.T.);
#9792=EDGE_CURVE('',#7638,#7639,#525,.T.);
#9793=EDGE_CURVE('',#7639,#7640,#526,.T.);
#9794=EDGE_CURVE('',#7641,#7640,#6248,.T.);
#9795=EDGE_CURVE('',#7641,#7642,#527,.T.);
#9796=EDGE_CURVE('',#7642,#7643,#528,.T.);
#9797=EDGE_CURVE('',#7644,#7643,#6249,.T.);
#9798=EDGE_CURVE('',#7644,#7645,#529,.T.);
#9799=EDGE_CURVE('',#7645,#7646,#530,.T.);
#9800=EDGE_CURVE('',#7647,#7646,#6250,.T.);
#9801=EDGE_CURVE('',#7647,#7648,#531,.T.);
#9802=EDGE_CURVE('',#7648,#7649,#532,.T.);
#9803=EDGE_CURVE('',#7650,#7649,#6251,.T.);
#9804=EDGE_CURVE('',#7650,#7651,#533,.T.);
#9805=EDGE_CURVE('',#7651,#7652,#534,.T.);
#9806=EDGE_CURVE('',#7653,#7652,#6252,.T.);
#9807=EDGE_CURVE('',#7653,#7654,#535,.T.);
#9808=EDGE_CURVE('',#7654,#7655,#536,.T.);
#9809=EDGE_CURVE('',#7656,#7655,#6253,.T.);
#9810=EDGE_CURVE('',#7656,#7657,#537,.T.);
#9811=EDGE_CURVE('',#7657,#7658,#538,.T.);
#9812=EDGE_CURVE('',#7659,#7658,#6254,.T.);
#9813=EDGE_CURVE('',#7659,#7660,#539,.T.);
#9814=EDGE_CURVE('',#7660,#7661,#540,.T.);
#9815=EDGE_CURVE('',#7662,#7661,#6255,.T.);
#9816=EDGE_CURVE('',#7662,#7663,#541,.T.);
#9817=EDGE_CURVE('',#7663,#7664,#542,.T.);
#9818=EDGE_CURVE('',#7665,#7664,#6256,.T.);
#9819=EDGE_CURVE('',#7665,#7666,#543,.T.);
#9820=EDGE_CURVE('',#7666,#7667,#544,.T.);
#9821=EDGE_CURVE('',#7668,#7667,#6257,.T.);
#9822=EDGE_CURVE('',#7668,#7669,#545,.T.);
#9823=EDGE_CURVE('',#7669,#7670,#546,.T.);
#9824=EDGE_CURVE('',#7671,#7670,#6258,.T.);
#9825=EDGE_CURVE('',#7671,#7672,#547,.T.);
#9826=EDGE_CURVE('',#7672,#7673,#548,.T.);
#9827=EDGE_CURVE('',#7674,#7673,#6259,.T.);
#9828=EDGE_CURVE('',#7674,#7675,#549,.T.);
#9829=EDGE_CURVE('',#7675,#7676,#550,.T.);
#9830=EDGE_CURVE('',#7677,#7676,#6260,.T.);
#9831=EDGE_CURVE('',#7677,#7445,#551,.T.);
#9832=EDGE_CURVE('',#7120,#7208,#4130,.T.);
#9833=EDGE_CURVE('',#7626,#7383,#4131,.T.);
#9834=EDGE_CURVE('',#7625,#7384,#4132,.T.);
#9835=EDGE_CURVE('',#7628,#7381,#4133,.T.);
#9836=EDGE_CURVE('',#7629,#7380,#4134,.T.);
#9837=EDGE_CURVE('',#7631,#7378,#4135,.T.);
#9838=EDGE_CURVE('',#7632,#7377,#4136,.T.);
#9839=EDGE_CURVE('',#7634,#7375,#4137,.T.);
#9840=EDGE_CURVE('',#7635,#7374,#4138,.T.);
#9841=EDGE_CURVE('',#7637,#7372,#4139,.T.);
#9842=EDGE_CURVE('',#7638,#7371,#4140,.T.);
#9843=EDGE_CURVE('',#7640,#7369,#4141,.T.);
#9844=EDGE_CURVE('',#7641,#7368,#4142,.T.);
#9845=EDGE_CURVE('',#7643,#7366,#4143,.T.);
#9846=EDGE_CURVE('',#7644,#7365,#4144,.T.);
#9847=EDGE_CURVE('',#7646,#7363,#4145,.T.);
#9848=EDGE_CURVE('',#7647,#7362,#4146,.T.);
#9849=EDGE_CURVE('',#7649,#7360,#4147,.T.);
#9850=EDGE_CURVE('',#7650,#7359,#4148,.T.);
#9851=EDGE_CURVE('',#7652,#7357,#4149,.T.);
#9852=EDGE_CURVE('',#7653,#7356,#4150,.T.);
#9853=EDGE_CURVE('',#7655,#7354,#4151,.T.);
#9854=EDGE_CURVE('',#7656,#7353,#4152,.T.);
#9855=EDGE_CURVE('',#7658,#7351,#4153,.T.);
#9856=EDGE_CURVE('',#7659,#7350,#4154,.T.);
#9857=EDGE_CURVE('',#7661,#7348,#4155,.T.);
#9858=EDGE_CURVE('',#7662,#7347,#4156,.T.);
#9859=EDGE_CURVE('',#7664,#7345,#4157,.T.);
#9860=EDGE_CURVE('',#7665,#7344,#4158,.T.);
#9861=EDGE_CURVE('',#7667,#7342,#4159,.T.);
#9862=EDGE_CURVE('',#7668,#7341,#4160,.T.);
#9863=EDGE_CURVE('',#7670,#7339,#4161,.T.);
#9864=EDGE_CURVE('',#7671,#7338,#4162,.T.);
#9865=EDGE_CURVE('',#7673,#7336,#4163,.T.);
#9866=EDGE_CURVE('',#7674,#7335,#4164,.T.);
#9867=EDGE_CURVE('',#7676,#7333,#4165,.T.);
#9868=EDGE_CURVE('',#7677,#7332,#4166,.T.);
#9869=EDGE_CURVE('',#7446,#7328,#4167,.T.);
#9870=EDGE_CURVE('',#7447,#7327,#4168,.T.);
#9871=EDGE_CURVE('',#7449,#7325,#4169,.T.);
#9872=EDGE_CURVE('',#7450,#7324,#4170,.T.);
#9873=EDGE_CURVE('',#7452,#7322,#4171,.T.);
#9874=EDGE_CURVE('',#7453,#7321,#4172,.T.);
#9875=EDGE_CURVE('',#7455,#7319,#4173,.T.);
#9876=EDGE_CURVE('',#7456,#7318,#4174,.T.);
#9877=EDGE_CURVE('',#7458,#7316,#4175,.T.);
#9878=EDGE_CURVE('',#7459,#7315,#4176,.T.);
#9879=EDGE_CURVE('',#7461,#7313,#4177,.T.);
#9880=EDGE_CURVE('',#7462,#7312,#4178,.T.);
#9881=EDGE_CURVE('',#7464,#7310,#4179,.T.);
#9882=EDGE_CURVE('',#7465,#7309,#4180,.T.);
#9883=EDGE_CURVE('',#7467,#7307,#4181,.T.);
#9884=EDGE_CURVE('',#7468,#7306,#4182,.T.);
#9885=EDGE_CURVE('',#7470,#7304,#4183,.T.);
#9886=EDGE_CURVE('',#7471,#7303,#4184,.T.);
#9887=EDGE_CURVE('',#7473,#7301,#4185,.T.);
#9888=EDGE_CURVE('',#7474,#7300,#4186,.T.);
#9889=EDGE_CURVE('',#7476,#7298,#4187,.T.);
#9890=EDGE_CURVE('',#7477,#7297,#4188,.T.);
#9891=EDGE_CURVE('',#7479,#7295,#4189,.T.);
#9892=EDGE_CURVE('',#7480,#7294,#4190,.T.);
#9893=EDGE_CURVE('',#7482,#7292,#4191,.T.);
#9894=EDGE_CURVE('',#7483,#7291,#4192,.T.);
#9895=EDGE_CURVE('',#7485,#7289,#4193,.T.);
#9896=EDGE_CURVE('',#7486,#7288,#4194,.T.);
#9897=EDGE_CURVE('',#7488,#7286,#4195,.T.);
#9898=EDGE_CURVE('',#7489,#7285,#4196,.T.);
#9899=EDGE_CURVE('',#7491,#7283,#4197,.T.);
#9900=EDGE_CURVE('',#7492,#7282,#4198,.T.);
#9901=EDGE_CURVE('',#7494,#7280,#4199,.T.);
#9902=EDGE_CURVE('',#7495,#7279,#4200,.T.);
#9903=EDGE_CURVE('',#7497,#7277,#4201,.T.);
#9904=EDGE_CURVE('',#7498,#7276,#4202,.T.);
#9905=EDGE_CURVE('',#7500,#7274,#4203,.T.);
#9906=EDGE_CURVE('',#7501,#7273,#4204,.T.);
#9907=EDGE_CURVE('',#7503,#7271,#4205,.T.);
#9908=EDGE_CURVE('',#7504,#7270,#4206,.T.);
#9909=EDGE_CURVE('',#7506,#7268,#4207,.T.);
#9910=EDGE_CURVE('',#7507,#7267,#4208,.T.);
#9911=EDGE_CURVE('',#7509,#7265,#4209,.T.);
#9912=EDGE_CURVE('',#7510,#7264,#4210,.T.);
#9913=EDGE_CURVE('',#7512,#7262,#4211,.T.);
#9914=EDGE_CURVE('',#7513,#7261,#4212,.T.);
#9915=EDGE_CURVE('',#7515,#7259,#4213,.T.);
#9916=EDGE_CURVE('',#7516,#7258,#4214,.T.);
#9917=EDGE_CURVE('',#7518,#7256,#4215,.T.);
#9918=EDGE_CURVE('',#7519,#7255,#4216,.T.);
#9919=EDGE_CURVE('',#7521,#7253,#4217,.T.);
#9920=EDGE_CURVE('',#7522,#7252,#4218,.T.);
#9921=EDGE_CURVE('',#7524,#7250,#4219,.T.);
#9922=EDGE_CURVE('',#7525,#7249,#4220,.T.);
#9923=EDGE_CURVE('',#7527,#7247,#4221,.T.);
#9924=EDGE_CURVE('',#7528,#7246,#4222,.T.);
#9925=EDGE_CURVE('',#7530,#7244,#4223,.T.);
#9926=EDGE_CURVE('',#7531,#7243,#4224,.T.);
#9927=EDGE_CURVE('',#7533,#7241,#4225,.T.);
#9928=EDGE_CURVE('',#7534,#7240,#4226,.T.);
#9929=EDGE_CURVE('',#7536,#7238,#4227,.T.);
#9930=EDGE_CURVE('',#7537,#7237,#4228,.T.);
#9931=EDGE_CURVE('',#7539,#7235,#4229,.T.);
#9932=EDGE_CURVE('',#7540,#7234,#4230,.T.);
#9933=EDGE_CURVE('',#7542,#7232,#4231,.T.);
#9934=EDGE_CURVE('',#7543,#7231,#4232,.T.);
#9935=EDGE_CURVE('',#7545,#7229,#4233,.T.);
#9936=EDGE_CURVE('',#7546,#7228,#4234,.T.);
#9937=EDGE_CURVE('',#7548,#7226,#4235,.T.);
#9938=EDGE_CURVE('',#7549,#7225,#4236,.T.);
#9939=EDGE_CURVE('',#7551,#7223,#4237,.T.);
#9940=EDGE_CURVE('',#7552,#7222,#4238,.T.);
#9941=EDGE_CURVE('',#7554,#7220,#4239,.T.);
#9942=EDGE_CURVE('',#7555,#7219,#4240,.T.);
#9943=EDGE_CURVE('',#7557,#7217,#4241,.T.);
#9944=EDGE_CURVE('',#7558,#7216,#4242,.T.);
#9945=EDGE_CURVE('',#7560,#7214,#4243,.T.);
#9946=EDGE_CURVE('',#7561,#7212,#4244,.T.);
#9947=EDGE_CURVE('',#7565,#7444,#4245,.T.);
#9948=EDGE_CURVE('',#7566,#7443,#4246,.T.);
#9949=EDGE_CURVE('',#7568,#7441,#4247,.T.);
#9950=EDGE_CURVE('',#7569,#7440,#4248,.T.);
#9951=EDGE_CURVE('',#7571,#7438,#4249,.T.);
#9952=EDGE_CURVE('',#7572,#7437,#4250,.T.);
#9953=EDGE_CURVE('',#7574,#7435,#4251,.T.);
#9954=EDGE_CURVE('',#7575,#7434,#4252,.T.);
#9955=EDGE_CURVE('',#7577,#7432,#4253,.T.);
#9956=EDGE_CURVE('',#7578,#7431,#4254,.T.);
#9957=EDGE_CURVE('',#7580,#7429,#4255,.T.);
#9958=EDGE_CURVE('',#7581,#7428,#4256,.T.);
#9959=EDGE_CURVE('',#7583,#7426,#4257,.T.);
#9960=EDGE_CURVE('',#7584,#7425,#4258,.T.);
#9961=EDGE_CURVE('',#7586,#7423,#4259,.T.);
#9962=EDGE_CURVE('',#7587,#7422,#4260,.T.);
#9963=EDGE_CURVE('',#7589,#7420,#4261,.T.);
#9964=EDGE_CURVE('',#7590,#7419,#4262,.T.);
#9965=EDGE_CURVE('',#7592,#7417,#4263,.T.);
#9966=EDGE_CURVE('',#7593,#7416,#4264,.T.);
#9967=EDGE_CURVE('',#7595,#7414,#4265,.T.);
#9968=EDGE_CURVE('',#7596,#7413,#4266,.T.);
#9969=EDGE_CURVE('',#7598,#7411,#4267,.T.);
#9970=EDGE_CURVE('',#7599,#7410,#4268,.T.);
#9971=EDGE_CURVE('',#7601,#7408,#4269,.T.);
#9972=EDGE_CURVE('',#7602,#7407,#4270,.T.);
#9973=EDGE_CURVE('',#7604,#7405,#4271,.T.);
#9974=EDGE_CURVE('',#7605,#7404,#4272,.T.);
#9975=EDGE_CURVE('',#7607,#7402,#4273,.T.);
#9976=EDGE_CURVE('',#7608,#7401,#4274,.T.);
#9977=EDGE_CURVE('',#7610,#7399,#4275,.T.);
#9978=EDGE_CURVE('',#7611,#7398,#4276,.T.);
#9979=EDGE_CURVE('',#7613,#7396,#4277,.T.);
#9980=EDGE_CURVE('',#7614,#7395,#4278,.T.);
#9981=EDGE_CURVE('',#7616,#7393,#4279,.T.);
#9982=EDGE_CURVE('',#7617,#7392,#4280,.T.);
#9983=EDGE_CURVE('',#7623,#7386,#4281,.T.);
#9984=EDGE_CURVE('',#7622,#7387,#4282,.T.);
#9985=EDGE_CURVE('',#7619,#7390,#4283,.T.);
#9986=EDGE_CURVE('',#7620,#7389,#4284,.T.);
#9987=EDGE_CURVE('',#7621,#7388,#4285,.T.);
#9988=EDGE_CURVE('',#7624,#7385,#4286,.T.);
#9989=EDGE_CURVE('',#7618,#7391,#4287,.T.);
#9990=EDGE_CURVE('',#7615,#7394,#4288,.T.);
#9991=EDGE_CURVE('',#7612,#7397,#4289,.T.);
#9992=EDGE_CURVE('',#7609,#7400,#4290,.T.);
#9993=EDGE_CURVE('',#7606,#7403,#4291,.T.);
#9994=EDGE_CURVE('',#7603,#7406,#4292,.T.);
#9995=EDGE_CURVE('',#7600,#7409,#4293,.T.);
#9996=EDGE_CURVE('',#7597,#7412,#4294,.T.);
#9997=EDGE_CURVE('',#7594,#7415,#4295,.T.);
#9998=EDGE_CURVE('',#7591,#7418,#4296,.T.);
#9999=EDGE_CURVE('',#7588,#7421,#4297,.T.);
#10000=EDGE_CURVE('',#7585,#7424,#4298,.T.);
#10001=EDGE_CURVE('',#7582,#7427,#4299,.T.);
#10002=EDGE_CURVE('',#7579,#7430,#4300,.T.);
#10003=EDGE_CURVE('',#7576,#7433,#4301,.T.);
#10004=EDGE_CURVE('',#7573,#7436,#4302,.T.);
#10005=EDGE_CURVE('',#7570,#7439,#4303,.T.);
#10006=EDGE_CURVE('',#7567,#7442,#4304,.T.);
#10007=EDGE_CURVE('',#7564,#7213,#4305,.T.);
#10008=EDGE_CURVE('',#7559,#7215,#4306,.T.);
#10009=EDGE_CURVE('',#7556,#7218,#4307,.T.);
#10010=EDGE_CURVE('',#7553,#7221,#4308,.T.);
#10011=EDGE_CURVE('',#7550,#7224,#4309,.T.);
#10012=EDGE_CURVE('',#7547,#7227,#4310,.T.);
#10013=EDGE_CURVE('',#7544,#7230,#4311,.T.);
#10014=EDGE_CURVE('',#7541,#7233,#4312,.T.);
#10015=EDGE_CURVE('',#7538,#7236,#4313,.T.);
#10016=EDGE_CURVE('',#7535,#7239,#4314,.T.);
#10017=EDGE_CURVE('',#7532,#7242,#4315,.T.);
#10018=EDGE_CURVE('',#7529,#7245,#4316,.T.);
#10019=EDGE_CURVE('',#7526,#7248,#4317,.T.);
#10020=EDGE_CURVE('',#7523,#7251,#4318,.T.);
#10021=EDGE_CURVE('',#7520,#7254,#4319,.T.);
#10022=EDGE_CURVE('',#7517,#7257,#4320,.T.);
#10023=EDGE_CURVE('',#7514,#7260,#4321,.T.);
#10024=EDGE_CURVE('',#7511,#7263,#4322,.T.);
#10025=EDGE_CURVE('',#7508,#7266,#4323,.T.);
#10026=EDGE_CURVE('',#7505,#7269,#4324,.T.);
#10027=EDGE_CURVE('',#7502,#7272,#4325,.T.);
#10028=EDGE_CURVE('',#7499,#7275,#4326,.T.);
#10029=EDGE_CURVE('',#7496,#7278,#4327,.T.);
#10030=EDGE_CURVE('',#7493,#7281,#4328,.T.);
#10031=EDGE_CURVE('',#7490,#7284,#4329,.T.);
#10032=EDGE_CURVE('',#7487,#7287,#4330,.T.);
#10033=EDGE_CURVE('',#7484,#7290,#4331,.T.);
#10034=EDGE_CURVE('',#7481,#7293,#4332,.T.);
#10035=EDGE_CURVE('',#7478,#7296,#4333,.T.);
#10036=EDGE_CURVE('',#7475,#7299,#4334,.T.);
#10037=EDGE_CURVE('',#7472,#7302,#4335,.T.);
#10038=EDGE_CURVE('',#7469,#7305,#4336,.T.);
#10039=EDGE_CURVE('',#7466,#7308,#4337,.T.);
#10040=EDGE_CURVE('',#7463,#7311,#4338,.T.);
#10041=EDGE_CURVE('',#7460,#7314,#4339,.T.);
#10042=EDGE_CURVE('',#7457,#7317,#4340,.T.);
#10043=EDGE_CURVE('',#7454,#7320,#4341,.T.);
#10044=EDGE_CURVE('',#7451,#7323,#4342,.T.);
#10045=EDGE_CURVE('',#7448,#7326,#4343,.T.);
#10046=EDGE_CURVE('',#7445,#7331,#4344,.T.);
#10047=EDGE_CURVE('',#7675,#7334,#4345,.T.);
#10048=EDGE_CURVE('',#7672,#7337,#4346,.T.);
#10049=EDGE_CURVE('',#7669,#7340,#4347,.T.);
#10050=EDGE_CURVE('',#7666,#7343,#4348,.T.);
#10051=EDGE_CURVE('',#7663,#7346,#4349,.T.);
#10052=EDGE_CURVE('',#7660,#7349,#4350,.T.);
#10053=EDGE_CURVE('',#7657,#7352,#4351,.T.);
#10054=EDGE_CURVE('',#7654,#7355,#4352,.T.);
#10055=EDGE_CURVE('',#7651,#7358,#4353,.T.);
#10056=EDGE_CURVE('',#7648,#7361,#4354,.T.);
#10057=EDGE_CURVE('',#7645,#7364,#4355,.T.);
#10058=EDGE_CURVE('',#7642,#7367,#4356,.T.);
#10059=EDGE_CURVE('',#7639,#7370,#4357,.T.);
#10060=EDGE_CURVE('',#7636,#7373,#4358,.T.);
#10061=EDGE_CURVE('',#7633,#7376,#4359,.T.);
#10062=EDGE_CURVE('',#7630,#7379,#4360,.T.);
#10063=EDGE_CURVE('',#7627,#7382,#4361,.T.);
#10064=EDGE_CURVE('',#7678,#7679,#6261,.T.);
#10065=EDGE_CURVE('',#7680,#7679,#1014,.T.);
#10066=EDGE_CURVE('',#7681,#7680,#6262,.T.);
#10067=EDGE_CURVE('',#7682,#7681,#1015,.T.);
#10068=EDGE_CURVE('',#7682,#7683,#6263,.T.);
#10069=EDGE_CURVE('',#7683,#7684,#6264,.T.);
#10070=EDGE_CURVE('',#7685,#7684,#6265,.T.);
#10071=EDGE_CURVE('',#7684,#7685,#6266,.T.);
#10072=EDGE_CURVE('',#7683,#7686,#6267,.T.);
#10073=EDGE_CURVE('',#7687,#7686,#1016,.T.);
#10074=EDGE_CURVE('',#7688,#7687,#6268,.T.);
#10075=EDGE_CURVE('',#7678,#7688,#1017,.T.);
#10076=EDGE_CURVE('',#7689,#7689,#6269,.T.);
#10077=EDGE_CURVE('',#7689,#7685,#4362,.T.);
#10078=EDGE_CURVE('',#7690,#7690,#6270,.T.);
#10079=EDGE_CURVE('',#7690,#7691,#4363,.T.);
#10080=EDGE_CURVE('',#7691,#7691,#6271,.T.);
#10081=EDGE_CURVE('',#7688,#7687,#4364,.T.);
#10082=EDGE_CURVE('',#7681,#7680,#4365,.T.);
#10083=EDGE_CURVE('',#7678,#7686,#4366,.T.);
#10084=EDGE_CURVE('',#7682,#7679,#4367,.T.);
#10085=EDGE_CURVE('',#7692,#7692,#6272,.T.);
#10086=EDGE_CURVE('',#7692,#7693,#6273,.T.);
#10087=EDGE_CURVE('',#7693,#7693,#6274,.T.);
#10088=EDGE_CURVE('',#7694,#7695,#6275,.T.);
#10089=EDGE_CURVE('',#7695,#7694,#6276,.T.);
#10090=EDGE_CURVE('',#7695,#7696,#4368,.T.);
#10091=EDGE_CURVE('',#7696,#7696,#6277,.T.);
#10092=EDGE_CURVE('',#7697,#7698,#6278,.T.);
#10093=EDGE_CURVE('',#7698,#7697,#6279,.T.);
#10094=EDGE_CURVE('',#7698,#7699,#4369,.T.);
#10095=EDGE_CURVE('',#7699,#7700,#6280,.T.);
#10096=EDGE_CURVE('',#7700,#7699,#6281,.T.);
#10097=EDGE_CURVE('',#7694,#7700,#4370,.T.);
#10098=EDGE_CURVE('',#7701,#7702,#6282,.T.);
#10099=EDGE_CURVE('',#7702,#7701,#6283,.T.);
#10100=EDGE_CURVE('',#7702,#7697,#4371,.T.);
#10101=EDGE_CURVE('',#7703,#7704,#6284,.T.);
#10102=EDGE_CURVE('',#7704,#7703,#6285,.T.);
#10103=EDGE_CURVE('',#7704,#7705,#4372,.T.);
#10104=EDGE_CURVE('',#7705,#7706,#6286,.T.);
#10105=EDGE_CURVE('',#7706,#7705,#6287,.T.);
#10106=EDGE_CURVE('',#7701,#7706,#4373,.T.);
#10107=EDGE_CURVE('',#7707,#7708,#6288,.T.);
#10108=EDGE_CURVE('',#7708,#7707,#6289,.T.);
#10109=EDGE_CURVE('',#7708,#7703,#4374,.T.);
#10110=EDGE_CURVE('',#7709,#7710,#6290,.T.);
#10111=EDGE_CURVE('',#7710,#7709,#6291,.T.);
#10112=EDGE_CURVE('',#7710,#7711,#4375,.T.);
#10113=EDGE_CURVE('',#7711,#7712,#6292,.T.);
#10114=EDGE_CURVE('',#7712,#7711,#6293,.T.);
#10115=EDGE_CURVE('',#7707,#7712,#4376,.T.);
#10116=EDGE_CURVE('',#7713,#7714,#6294,.T.);
#10117=EDGE_CURVE('',#7714,#7713,#6295,.T.);
#10118=EDGE_CURVE('',#7714,#7709,#4377,.T.);
#10119=EDGE_CURVE('',#7715,#7716,#6296,.T.);
#10120=EDGE_CURVE('',#7716,#7715,#6297,.T.);
#10121=EDGE_CURVE('',#7716,#7717,#4378,.T.);
#10122=EDGE_CURVE('',#7717,#7718,#6298,.T.);
#10123=EDGE_CURVE('',#7718,#7717,#6299,.T.);
#10124=EDGE_CURVE('',#7713,#7718,#4379,.T.);
#10125=EDGE_CURVE('',#7719,#7720,#6300,.T.);
#10126=EDGE_CURVE('',#7720,#7719,#6301,.T.);
#10127=EDGE_CURVE('',#7720,#7715,#4380,.T.);
#10128=EDGE_CURVE('',#7721,#7722,#6302,.T.);
#10129=EDGE_CURVE('',#7722,#7721,#6303,.T.);
#10130=EDGE_CURVE('',#7722,#7723,#4381,.T.);
#10131=EDGE_CURVE('',#7723,#7724,#6304,.T.);
#10132=EDGE_CURVE('',#7724,#7723,#6305,.T.);
#10133=EDGE_CURVE('',#7719,#7724,#4382,.T.);
#10134=EDGE_CURVE('',#7725,#7726,#6306,.T.);
#10135=EDGE_CURVE('',#7726,#7725,#6307,.T.);
#10136=EDGE_CURVE('',#7726,#7721,#4383,.T.);
#10137=EDGE_CURVE('',#7727,#7728,#6308,.T.);
#10138=EDGE_CURVE('',#7728,#7727,#6309,.T.);
#10139=EDGE_CURVE('',#7728,#7729,#4384,.T.);
#10140=EDGE_CURVE('',#7729,#7730,#6310,.T.);
#10141=EDGE_CURVE('',#7730,#7729,#6311,.T.);
#10142=EDGE_CURVE('',#7725,#7730,#4385,.T.);
#10143=EDGE_CURVE('',#7731,#7732,#6312,.T.);
#10144=EDGE_CURVE('',#7732,#7731,#6313,.T.);
#10145=EDGE_CURVE('',#7732,#7727,#4386,.T.);
#10146=EDGE_CURVE('',#7733,#7734,#6314,.T.);
#10147=EDGE_CURVE('',#7734,#7733,#6315,.T.);
#10148=EDGE_CURVE('',#7734,#7735,#4387,.T.);
#10149=EDGE_CURVE('',#7735,#7736,#6316,.T.);
#10150=EDGE_CURVE('',#7736,#7735,#6317,.T.);
#10151=EDGE_CURVE('',#7731,#7736,#4388,.T.);
#10152=EDGE_CURVE('',#7737,#7738,#6318,.T.);
#10153=EDGE_CURVE('',#7738,#7737,#6319,.T.);
#10154=EDGE_CURVE('',#7738,#7733,#4389,.T.);
#10155=EDGE_CURVE('',#7739,#7740,#6320,.T.);
#10156=EDGE_CURVE('',#7740,#7739,#6321,.T.);
#10157=EDGE_CURVE('',#7740,#7741,#4390,.T.);
#10158=EDGE_CURVE('',#7741,#7742,#6322,.T.);
#10159=EDGE_CURVE('',#7742,#7741,#6323,.T.);
#10160=EDGE_CURVE('',#7737,#7742,#4391,.T.);
#10161=EDGE_CURVE('',#7743,#7744,#6324,.T.);
#10162=EDGE_CURVE('',#7744,#7743,#6325,.T.);
#10163=EDGE_CURVE('',#7744,#7739,#4392,.T.);
#10164=EDGE_CURVE('',#7745,#7746,#6326,.T.);
#10165=EDGE_CURVE('',#7746,#7745,#6327,.T.);
#10166=EDGE_CURVE('',#7746,#7747,#4393,.T.);
#10167=EDGE_CURVE('',#7747,#7748,#6328,.T.);
#10168=EDGE_CURVE('',#7748,#7747,#6329,.T.);
#10169=EDGE_CURVE('',#7743,#7748,#4394,.T.);
#10170=EDGE_CURVE('',#7749,#7750,#6330,.T.);
#10171=EDGE_CURVE('',#7750,#7749,#6331,.T.);
#10172=EDGE_CURVE('',#7750,#7745,#4395,.T.);
#10173=EDGE_CURVE('',#7751,#7752,#6332,.T.);
#10174=EDGE_CURVE('',#7752,#7751,#6333,.T.);
#10175=EDGE_CURVE('',#7752,#7753,#4396,.T.);
#10176=EDGE_CURVE('',#7753,#7754,#6334,.T.);
#10177=EDGE_CURVE('',#7754,#7753,#6335,.T.);
#10178=EDGE_CURVE('',#7749,#7754,#4397,.T.);
#10179=EDGE_CURVE('',#7755,#7756,#6336,.T.);
#10180=EDGE_CURVE('',#7756,#7755,#6337,.T.);
#10181=EDGE_CURVE('',#7756,#7751,#4398,.T.);
#10182=EDGE_CURVE('',#7757,#7758,#6338,.T.);
#10183=EDGE_CURVE('',#7758,#7757,#6339,.T.);
#10184=EDGE_CURVE('',#7758,#7759,#4399,.T.);
#10185=EDGE_CURVE('',#7759,#7760,#6340,.T.);
#10186=EDGE_CURVE('',#7760,#7759,#6341,.T.);
#10187=EDGE_CURVE('',#7755,#7760,#4400,.T.);
#10188=EDGE_CURVE('',#7761,#7762,#6342,.T.);
#10189=EDGE_CURVE('',#7762,#7761,#6343,.T.);
#10190=EDGE_CURVE('',#7762,#7757,#4401,.T.);
#10191=EDGE_CURVE('',#7763,#7764,#6344,.T.);
#10192=EDGE_CURVE('',#7764,#7763,#6345,.T.);
#10193=EDGE_CURVE('',#7764,#7765,#4402,.T.);
#10194=EDGE_CURVE('',#7765,#7766,#6346,.T.);
#10195=EDGE_CURVE('',#7766,#7765,#6347,.T.);
#10196=EDGE_CURVE('',#7761,#7766,#4403,.T.);
#10197=EDGE_CURVE('',#7767,#7768,#6348,.T.);
#10198=EDGE_CURVE('',#7768,#7767,#6349,.T.);
#10199=EDGE_CURVE('',#7768,#7763,#4404,.T.);
#10200=EDGE_CURVE('',#7769,#7770,#6350,.T.);
#10201=EDGE_CURVE('',#7770,#7769,#6351,.T.);
#10202=EDGE_CURVE('',#7770,#7771,#4405,.T.);
#10203=EDGE_CURVE('',#7771,#7772,#6352,.T.);
#10204=EDGE_CURVE('',#7772,#7771,#6353,.T.);
#10205=EDGE_CURVE('',#7767,#7772,#4406,.T.);
#10206=EDGE_CURVE('',#7693,#7773,#4407,.T.);
#10207=EDGE_CURVE('',#7773,#7773,#6354,.T.);
#10208=EDGE_CURVE('',#7774,#7775,#552,.F.);
#10209=EDGE_CURVE('',#7776,#7775,#6355,.T.);
#10210=EDGE_CURVE('',#7776,#7777,#553,.T.);
#10211=EDGE_CURVE('',#7777,#7778,#554,.T.);
#10212=EDGE_CURVE('',#7779,#7778,#6356,.T.);
#10213=EDGE_CURVE('',#7779,#7780,#555,.T.);
#10214=EDGE_CURVE('',#7780,#7781,#556,.T.);
#10215=EDGE_CURVE('',#7782,#7781,#6357,.T.);
#10216=EDGE_CURVE('',#7782,#7783,#557,.T.);
#10217=EDGE_CURVE('',#7783,#7784,#558,.T.);
#10218=EDGE_CURVE('',#7785,#7784,#6358,.T.);
#10219=EDGE_CURVE('',#7785,#7786,#559,.T.);
#10220=EDGE_CURVE('',#7786,#7787,#560,.T.);
#10221=EDGE_CURVE('',#7788,#7787,#6359,.T.);
#10222=EDGE_CURVE('',#7788,#7789,#561,.T.);
#10223=EDGE_CURVE('',#7789,#7790,#562,.T.);
#10224=EDGE_CURVE('',#7791,#7790,#6360,.T.);
#10225=EDGE_CURVE('',#7791,#7792,#563,.T.);
#10226=EDGE_CURVE('',#7792,#7793,#564,.T.);
#10227=EDGE_CURVE('',#7794,#7793,#6361,.T.);
#10228=EDGE_CURVE('',#7794,#7795,#565,.T.);
#10229=EDGE_CURVE('',#7795,#7796,#566,.T.);
#10230=EDGE_CURVE('',#7797,#7796,#6362,.T.);
#10231=EDGE_CURVE('',#7797,#7798,#567,.T.);
#10232=EDGE_CURVE('',#7798,#7799,#568,.T.);
#10233=EDGE_CURVE('',#7800,#7799,#6363,.T.);
#10234=EDGE_CURVE('',#7800,#7801,#569,.T.);
#10235=EDGE_CURVE('',#7801,#7802,#570,.T.);
#10236=EDGE_CURVE('',#7803,#7802,#6364,.T.);
#10237=EDGE_CURVE('',#7803,#7804,#571,.T.);
#10238=EDGE_CURVE('',#7804,#7805,#572,.T.);
#10239=EDGE_CURVE('',#7806,#7805,#6365,.T.);
#10240=EDGE_CURVE('',#7806,#7807,#573,.T.);
#10241=EDGE_CURVE('',#7807,#7808,#574,.T.);
#10242=EDGE_CURVE('',#7809,#7808,#6366,.T.);
#10243=EDGE_CURVE('',#7809,#7810,#575,.T.);
#10244=EDGE_CURVE('',#7810,#7811,#576,.T.);
#10245=EDGE_CURVE('',#7812,#7811,#6367,.T.);
#10246=EDGE_CURVE('',#7812,#7813,#577,.T.);
#10247=EDGE_CURVE('',#7813,#7814,#578,.T.);
#10248=EDGE_CURVE('',#7815,#7814,#6368,.T.);
#10249=EDGE_CURVE('',#7815,#7816,#579,.T.);
#10250=EDGE_CURVE('',#7816,#7817,#580,.T.);
#10251=EDGE_CURVE('',#7818,#7817,#6369,.T.);
#10252=EDGE_CURVE('',#7818,#7819,#581,.T.);
#10253=EDGE_CURVE('',#7819,#7820,#582,.T.);
#10254=EDGE_CURVE('',#7821,#7820,#6370,.T.);
#10255=EDGE_CURVE('',#7821,#7822,#583,.T.);
#10256=EDGE_CURVE('',#7822,#7823,#584,.T.);
#10257=EDGE_CURVE('',#7824,#7823,#6371,.T.);
#10258=EDGE_CURVE('',#7824,#7825,#585,.T.);
#10259=EDGE_CURVE('',#7825,#7826,#586,.T.);
#10260=EDGE_CURVE('',#7827,#7826,#6372,.T.);
#10261=EDGE_CURVE('',#7827,#7828,#587,.T.);
#10262=EDGE_CURVE('',#7828,#7829,#588,.T.);
#10263=EDGE_CURVE('',#7830,#7829,#6373,.T.);
#10264=EDGE_CURVE('',#7830,#7831,#589,.T.);
#10265=EDGE_CURVE('',#7831,#7832,#590,.T.);
#10266=EDGE_CURVE('',#7833,#7832,#6374,.T.);
#10267=EDGE_CURVE('',#7833,#7834,#591,.T.);
#10268=EDGE_CURVE('',#7834,#7835,#592,.T.);
#10269=EDGE_CURVE('',#7836,#7835,#6375,.T.);
#10270=EDGE_CURVE('',#7836,#7837,#593,.T.);
#10271=EDGE_CURVE('',#7837,#7838,#594,.T.);
#10272=EDGE_CURVE('',#7839,#7838,#6376,.T.);
#10273=EDGE_CURVE('',#7839,#7840,#595,.T.);
#10274=EDGE_CURVE('',#7840,#7841,#596,.T.);
#10275=EDGE_CURVE('',#7842,#7841,#6377,.T.);
#10276=EDGE_CURVE('',#7842,#7843,#597,.T.);
#10277=EDGE_CURVE('',#7843,#7844,#598,.T.);
#10278=EDGE_CURVE('',#7845,#7844,#6378,.T.);
#10279=EDGE_CURVE('',#7845,#7846,#599,.T.);
#10280=EDGE_CURVE('',#7846,#7847,#600,.T.);
#10281=EDGE_CURVE('',#7848,#7847,#6379,.T.);
#10282=EDGE_CURVE('',#7848,#7849,#601,.T.);
#10283=EDGE_CURVE('',#7849,#7850,#602,.T.);
#10284=EDGE_CURVE('',#7851,#7850,#6380,.T.);
#10285=EDGE_CURVE('',#7851,#7852,#603,.T.);
#10286=EDGE_CURVE('',#7852,#7853,#604,.T.);
#10287=EDGE_CURVE('',#7854,#7853,#6381,.T.);
#10288=EDGE_CURVE('',#7854,#7855,#605,.T.);
#10289=EDGE_CURVE('',#7855,#7856,#606,.T.);
#10290=EDGE_CURVE('',#7857,#7856,#6382,.T.);
#10291=EDGE_CURVE('',#7857,#7858,#607,.T.);
#10292=EDGE_CURVE('',#7858,#7859,#608,.T.);
#10293=EDGE_CURVE('',#7860,#7859,#6383,.T.);
#10294=EDGE_CURVE('',#7860,#7861,#609,.T.);
#10295=EDGE_CURVE('',#7861,#7862,#610,.T.);
#10296=EDGE_CURVE('',#7863,#7862,#6384,.T.);
#10297=EDGE_CURVE('',#7863,#7864,#611,.T.);
#10298=EDGE_CURVE('',#7864,#7865,#612,.T.);
#10299=EDGE_CURVE('',#7866,#7865,#6385,.T.);
#10300=EDGE_CURVE('',#7866,#7867,#613,.T.);
#10301=EDGE_CURVE('',#7867,#7868,#614,.T.);
#10302=EDGE_CURVE('',#7869,#7868,#6386,.T.);
#10303=EDGE_CURVE('',#7869,#7870,#615,.T.);
#10304=EDGE_CURVE('',#7870,#7871,#616,.T.);
#10305=EDGE_CURVE('',#7872,#7871,#6387,.T.);
#10306=EDGE_CURVE('',#7872,#7873,#617,.T.);
#10307=EDGE_CURVE('',#7873,#7874,#618,.T.);
#10308=EDGE_CURVE('',#7875,#7874,#6388,.T.);
#10309=EDGE_CURVE('',#7875,#7876,#619,.T.);
#10310=EDGE_CURVE('',#7876,#7877,#620,.T.);
#10311=EDGE_CURVE('',#7878,#7877,#6389,.T.);
#10312=EDGE_CURVE('',#7878,#7879,#621,.T.);
#10313=EDGE_CURVE('',#7879,#7880,#622,.T.);
#10314=EDGE_CURVE('',#7881,#7880,#6390,.T.);
#10315=EDGE_CURVE('',#7881,#7882,#623,.T.);
#10316=EDGE_CURVE('',#7882,#7883,#624,.T.);
#10317=EDGE_CURVE('',#7884,#7883,#6391,.T.);
#10318=EDGE_CURVE('',#7884,#7885,#625,.T.);
#10319=EDGE_CURVE('',#7885,#7886,#626,.T.);
#10320=EDGE_CURVE('',#7887,#7886,#6392,.T.);
#10321=EDGE_CURVE('',#7887,#7888,#627,.T.);
#10322=EDGE_CURVE('',#7888,#7889,#628,.T.);
#10323=EDGE_CURVE('',#7890,#7889,#6393,.T.);
#10324=EDGE_CURVE('',#7890,#7891,#629,.T.);
#10325=EDGE_CURVE('',#7891,#7892,#4408,.T.);
#10326=EDGE_CURVE('',#7892,#7892,#6394,.T.);
#10327=EDGE_CURVE('',#7891,#7893,#630,.T.);
#10328=EDGE_CURVE('',#7893,#7894,#631,.T.);
#10329=EDGE_CURVE('',#7895,#7894,#6395,.T.);
#10330=EDGE_CURVE('',#7895,#7896,#632,.T.);
#10331=EDGE_CURVE('',#7896,#7897,#633,.T.);
#10332=EDGE_CURVE('',#7898,#7897,#6396,.T.);
#10333=EDGE_CURVE('',#7898,#7899,#634,.T.);
#10334=EDGE_CURVE('',#7899,#7900,#635,.T.);
#10335=EDGE_CURVE('',#7901,#7900,#6397,.T.);
#10336=EDGE_CURVE('',#7901,#7902,#636,.T.);
#10337=EDGE_CURVE('',#7902,#7903,#637,.T.);
#10338=EDGE_CURVE('',#7904,#7903,#6398,.T.);
#10339=EDGE_CURVE('',#7904,#7905,#638,.T.);
#10340=EDGE_CURVE('',#7905,#7906,#639,.T.);
#10341=EDGE_CURVE('',#7907,#7906,#6399,.T.);
#10342=EDGE_CURVE('',#7907,#7908,#640,.T.);
#10343=EDGE_CURVE('',#7908,#7909,#641,.T.);
#10344=EDGE_CURVE('',#7910,#7909,#6400,.T.);
#10345=EDGE_CURVE('',#7910,#7911,#642,.T.);
#10346=EDGE_CURVE('',#7911,#7912,#643,.T.);
#10347=EDGE_CURVE('',#7913,#7912,#6401,.T.);
#10348=EDGE_CURVE('',#7913,#7914,#644,.T.);
#10349=EDGE_CURVE('',#7914,#7915,#645,.T.);
#10350=EDGE_CURVE('',#7916,#7915,#6402,.T.);
#10351=EDGE_CURVE('',#7916,#7917,#646,.T.);
#10352=EDGE_CURVE('',#7917,#7918,#647,.T.);
#10353=EDGE_CURVE('',#7919,#7918,#6403,.T.);
#10354=EDGE_CURVE('',#7919,#7920,#648,.T.);
#10355=EDGE_CURVE('',#7920,#7921,#649,.T.);
#10356=EDGE_CURVE('',#7922,#7921,#6404,.T.);
#10357=EDGE_CURVE('',#7922,#7923,#650,.T.);
#10358=EDGE_CURVE('',#7923,#7924,#651,.T.);
#10359=EDGE_CURVE('',#7925,#7924,#6405,.T.);
#10360=EDGE_CURVE('',#7925,#7926,#652,.T.);
#10361=EDGE_CURVE('',#7926,#7927,#653,.T.);
#10362=EDGE_CURVE('',#7928,#7927,#6406,.T.);
#10363=EDGE_CURVE('',#7928,#7929,#654,.T.);
#10364=EDGE_CURVE('',#7929,#7930,#655,.T.);
#10365=EDGE_CURVE('',#7931,#7930,#6407,.T.);
#10366=EDGE_CURVE('',#7931,#7932,#656,.T.);
#10367=EDGE_CURVE('',#7932,#7933,#657,.T.);
#10368=EDGE_CURVE('',#7934,#7933,#6408,.T.);
#10369=EDGE_CURVE('',#7934,#7935,#658,.T.);
#10370=EDGE_CURVE('',#7935,#7936,#659,.T.);
#10371=EDGE_CURVE('',#7937,#7936,#6409,.T.);
#10372=EDGE_CURVE('',#7937,#7938,#660,.T.);
#10373=EDGE_CURVE('',#7938,#7939,#661,.T.);
#10374=EDGE_CURVE('',#7940,#7939,#6410,.T.);
#10375=EDGE_CURVE('',#7940,#7941,#662,.T.);
#10376=EDGE_CURVE('',#7941,#7942,#663,.T.);
#10377=EDGE_CURVE('',#7943,#7942,#6411,.T.);
#10378=EDGE_CURVE('',#7943,#7944,#664,.T.);
#10379=EDGE_CURVE('',#7944,#7945,#665,.T.);
#10380=EDGE_CURVE('',#7946,#7945,#6412,.T.);
#10381=EDGE_CURVE('',#7946,#7947,#666,.T.);
#10382=EDGE_CURVE('',#7947,#7948,#667,.T.);
#10383=EDGE_CURVE('',#7949,#7948,#6413,.T.);
#10384=EDGE_CURVE('',#7949,#7950,#668,.T.);
#10385=EDGE_CURVE('',#7950,#7951,#669,.T.);
#10386=EDGE_CURVE('',#7952,#7951,#6414,.T.);
#10387=EDGE_CURVE('',#7952,#7953,#670,.T.);
#10388=EDGE_CURVE('',#7953,#7954,#671,.T.);
#10389=EDGE_CURVE('',#7955,#7954,#6415,.T.);
#10390=EDGE_CURVE('',#7955,#7956,#672,.T.);
#10391=EDGE_CURVE('',#7956,#7957,#673,.T.);
#10392=EDGE_CURVE('',#7958,#7957,#6416,.T.);
#10393=EDGE_CURVE('',#7958,#7959,#674,.T.);
#10394=EDGE_CURVE('',#7959,#7960,#675,.T.);
#10395=EDGE_CURVE('',#7961,#7960,#6417,.T.);
#10396=EDGE_CURVE('',#7961,#7962,#676,.T.);
#10397=EDGE_CURVE('',#7962,#7963,#677,.T.);
#10398=EDGE_CURVE('',#7964,#7963,#6418,.T.);
#10399=EDGE_CURVE('',#7964,#7965,#678,.T.);
#10400=EDGE_CURVE('',#7965,#7966,#679,.T.);
#10401=EDGE_CURVE('',#7967,#7966,#6419,.T.);
#10402=EDGE_CURVE('',#7967,#7968,#680,.T.);
#10403=EDGE_CURVE('',#7968,#7969,#681,.T.);
#10404=EDGE_CURVE('',#7970,#7969,#6420,.T.);
#10405=EDGE_CURVE('',#7970,#7971,#682,.T.);
#10406=EDGE_CURVE('',#7971,#7972,#683,.T.);
#10407=EDGE_CURVE('',#7973,#7972,#6421,.T.);
#10408=EDGE_CURVE('',#7973,#7974,#684,.T.);
#10409=EDGE_CURVE('',#7974,#7975,#685,.T.);
#10410=EDGE_CURVE('',#7976,#7975,#6422,.T.);
#10411=EDGE_CURVE('',#7976,#7977,#686,.T.);
#10412=EDGE_CURVE('',#7977,#7978,#687,.T.);
#10413=EDGE_CURVE('',#7979,#7978,#6423,.T.);
#10414=EDGE_CURVE('',#7979,#7980,#688,.T.);
#10415=EDGE_CURVE('',#7980,#7981,#689,.T.);
#10416=EDGE_CURVE('',#7982,#7981,#6424,.T.);
#10417=EDGE_CURVE('',#7982,#7983,#690,.T.);
#10418=EDGE_CURVE('',#7983,#7984,#691,.T.);
#10419=EDGE_CURVE('',#7985,#7984,#6425,.T.);
#10420=EDGE_CURVE('',#7985,#7986,#692,.T.);
#10421=EDGE_CURVE('',#7986,#7987,#693,.T.);
#10422=EDGE_CURVE('',#7988,#7987,#6426,.T.);
#10423=EDGE_CURVE('',#7988,#7989,#694,.T.);
#10424=EDGE_CURVE('',#7989,#7990,#695,.T.);
#10425=EDGE_CURVE('',#7991,#7990,#6427,.T.);
#10426=EDGE_CURVE('',#7991,#7992,#696,.T.);
#10427=EDGE_CURVE('',#7992,#7993,#697,.T.);
#10428=EDGE_CURVE('',#7994,#7993,#6428,.T.);
#10429=EDGE_CURVE('',#7994,#7995,#698,.T.);
#10430=EDGE_CURVE('',#7995,#7996,#699,.T.);
#10431=EDGE_CURVE('',#7997,#7996,#6429,.T.);
#10432=EDGE_CURVE('',#7997,#7998,#700,.T.);
#10433=EDGE_CURVE('',#7998,#7999,#701,.T.);
#10434=EDGE_CURVE('',#8000,#7999,#6430,.T.);
#10435=EDGE_CURVE('',#8000,#8001,#702,.T.);
#10436=EDGE_CURVE('',#8001,#8002,#703,.T.);
#10437=EDGE_CURVE('',#8003,#8002,#6431,.T.);
#10438=EDGE_CURVE('',#8003,#8004,#704,.T.);
#10439=EDGE_CURVE('',#8004,#8005,#705,.T.);
#10440=EDGE_CURVE('',#8006,#8005,#6432,.T.);
#10441=EDGE_CURVE('',#8006,#7774,#706,.T.);
#10442=EDGE_CURVE('',#8007,#8008,#707,.T.);
#10443=EDGE_CURVE('',#8007,#8009,#6433,.T.);
#10444=EDGE_CURVE('',#8010,#8009,#708,.T.);
#10445=EDGE_CURVE('',#8011,#8010,#709,.T.);
#10446=EDGE_CURVE('',#8011,#8012,#6434,.T.);
#10447=EDGE_CURVE('',#8013,#8012,#710,.T.);
#10448=EDGE_CURVE('',#8014,#8013,#711,.T.);
#10449=EDGE_CURVE('',#8014,#8015,#6435,.T.);
#10450=EDGE_CURVE('',#8016,#8015,#712,.T.);
#10451=EDGE_CURVE('',#8017,#8016,#713,.T.);
#10452=EDGE_CURVE('',#8017,#8018,#6436,.T.);
#10453=EDGE_CURVE('',#8019,#8018,#714,.T.);
#10454=EDGE_CURVE('',#8020,#8019,#715,.T.);
#10455=EDGE_CURVE('',#8020,#8021,#6437,.T.);
#10456=EDGE_CURVE('',#8022,#8021,#716,.T.);
#10457=EDGE_CURVE('',#8023,#8022,#717,.T.);
#10458=EDGE_CURVE('',#8023,#8024,#6438,.T.);
#10459=EDGE_CURVE('',#8025,#8024,#718,.T.);
#10460=EDGE_CURVE('',#8026,#8025,#719,.T.);
#10461=EDGE_CURVE('',#8026,#8027,#6439,.T.);
#10462=EDGE_CURVE('',#8028,#8027,#720,.T.);
#10463=EDGE_CURVE('',#8029,#8028,#721,.T.);
#10464=EDGE_CURVE('',#8029,#8030,#6440,.T.);
#10465=EDGE_CURVE('',#8031,#8030,#722,.T.);
#10466=EDGE_CURVE('',#8032,#8031,#723,.T.);
#10467=EDGE_CURVE('',#8032,#8033,#6441,.T.);
#10468=EDGE_CURVE('',#8034,#8033,#724,.T.);
#10469=EDGE_CURVE('',#8035,#8034,#725,.T.);
#10470=EDGE_CURVE('',#8035,#8036,#6442,.T.);
#10471=EDGE_CURVE('',#8037,#8036,#726,.T.);
#10472=EDGE_CURVE('',#8038,#8037,#727,.T.);
#10473=EDGE_CURVE('',#8038,#8039,#6443,.T.);
#10474=EDGE_CURVE('',#8040,#8039,#728,.T.);
#10475=EDGE_CURVE('',#8041,#8040,#729,.T.);
#10476=EDGE_CURVE('',#8041,#8042,#6444,.T.);
#10477=EDGE_CURVE('',#8043,#8042,#730,.T.);
#10478=EDGE_CURVE('',#8044,#8043,#731,.T.);
#10479=EDGE_CURVE('',#8044,#8045,#6445,.T.);
#10480=EDGE_CURVE('',#8046,#8045,#732,.T.);
#10481=EDGE_CURVE('',#8047,#8046,#733,.T.);
#10482=EDGE_CURVE('',#8047,#8048,#6446,.T.);
#10483=EDGE_CURVE('',#8049,#8048,#734,.T.);
#10484=EDGE_CURVE('',#8050,#8049,#735,.T.);
#10485=EDGE_CURVE('',#8050,#8051,#6447,.T.);
#10486=EDGE_CURVE('',#8052,#8051,#736,.T.);
#10487=EDGE_CURVE('',#8053,#8052,#737,.T.);
#10488=EDGE_CURVE('',#8053,#8054,#6448,.T.);
#10489=EDGE_CURVE('',#8055,#8054,#738,.T.);
#10490=EDGE_CURVE('',#8056,#8055,#739,.T.);
#10491=EDGE_CURVE('',#8056,#8057,#6449,.T.);
#10492=EDGE_CURVE('',#8058,#8057,#740,.T.);
#10493=EDGE_CURVE('',#8059,#8058,#741,.T.);
#10494=EDGE_CURVE('',#8059,#8060,#6450,.T.);
#10495=EDGE_CURVE('',#8061,#8060,#742,.T.);
#10496=EDGE_CURVE('',#8062,#8061,#743,.T.);
#10497=EDGE_CURVE('',#8062,#8063,#6451,.T.);
#10498=EDGE_CURVE('',#8064,#8063,#744,.T.);
#10499=EDGE_CURVE('',#8065,#8064,#745,.T.);
#10500=EDGE_CURVE('',#8065,#8066,#6452,.T.);
#10501=EDGE_CURVE('',#8067,#8066,#746,.T.);
#10502=EDGE_CURVE('',#8068,#8067,#747,.T.);
#10503=EDGE_CURVE('',#8068,#8069,#6453,.T.);
#10504=EDGE_CURVE('',#8070,#8069,#748,.T.);
#10505=EDGE_CURVE('',#8071,#8070,#749,.T.);
#10506=EDGE_CURVE('',#8071,#8072,#6454,.T.);
#10507=EDGE_CURVE('',#8073,#8072,#750,.T.);
#10508=EDGE_CURVE('',#8074,#8073,#751,.T.);
#10509=EDGE_CURVE('',#8074,#8075,#6455,.T.);
#10510=EDGE_CURVE('',#8076,#8075,#752,.T.);
#10511=EDGE_CURVE('',#8077,#8076,#753,.T.);
#10512=EDGE_CURVE('',#8077,#8078,#6456,.T.);
#10513=EDGE_CURVE('',#8079,#8078,#754,.T.);
#10514=EDGE_CURVE('',#8080,#8079,#755,.T.);
#10515=EDGE_CURVE('',#8080,#8081,#6457,.T.);
#10516=EDGE_CURVE('',#8082,#8081,#756,.T.);
#10517=EDGE_CURVE('',#8083,#8082,#757,.T.);
#10518=EDGE_CURVE('',#8083,#8084,#6458,.T.);
#10519=EDGE_CURVE('',#8085,#8084,#758,.T.);
#10520=EDGE_CURVE('',#8086,#8085,#759,.T.);
#10521=EDGE_CURVE('',#8086,#8087,#6459,.T.);
#10522=EDGE_CURVE('',#8088,#8087,#760,.T.);
#10523=EDGE_CURVE('',#8089,#8088,#761,.T.);
#10524=EDGE_CURVE('',#8089,#8090,#6460,.T.);
#10525=EDGE_CURVE('',#8091,#8090,#762,.T.);
#10526=EDGE_CURVE('',#8092,#8091,#763,.T.);
#10527=EDGE_CURVE('',#8092,#8093,#6461,.T.);
#10528=EDGE_CURVE('',#8094,#8093,#764,.T.);
#10529=EDGE_CURVE('',#8095,#8094,#765,.T.);
#10530=EDGE_CURVE('',#8095,#8096,#6462,.T.);
#10531=EDGE_CURVE('',#8097,#8096,#766,.T.);
#10532=EDGE_CURVE('',#8098,#8097,#767,.T.);
#10533=EDGE_CURVE('',#8098,#8099,#6463,.T.);
#10534=EDGE_CURVE('',#8100,#8099,#768,.T.);
#10535=EDGE_CURVE('',#8101,#8100,#769,.T.);
#10536=EDGE_CURVE('',#8101,#8102,#6464,.T.);
#10537=EDGE_CURVE('',#8103,#8102,#770,.T.);
#10538=EDGE_CURVE('',#8104,#8103,#771,.T.);
#10539=EDGE_CURVE('',#8104,#8105,#6465,.T.);
#10540=EDGE_CURVE('',#8106,#8105,#772,.T.);
#10541=EDGE_CURVE('',#8107,#8106,#773,.T.);
#10542=EDGE_CURVE('',#8107,#8108,#6466,.T.);
#10543=EDGE_CURVE('',#8109,#8108,#774,.T.);
#10544=EDGE_CURVE('',#8110,#8109,#775,.T.);
#10545=EDGE_CURVE('',#8110,#8111,#6467,.T.);
#10546=EDGE_CURVE('',#8112,#8111,#776,.T.);
#10547=EDGE_CURVE('',#8113,#8112,#777,.T.);
#10548=EDGE_CURVE('',#8113,#8114,#6468,.T.);
#10549=EDGE_CURVE('',#8115,#8114,#778,.T.);
#10550=EDGE_CURVE('',#8116,#8115,#779,.T.);
#10551=EDGE_CURVE('',#8116,#8117,#6469,.T.);
#10552=EDGE_CURVE('',#8118,#8117,#780,.T.);
#10553=EDGE_CURVE('',#8119,#8118,#781,.T.);
#10554=EDGE_CURVE('',#8119,#8120,#6470,.T.);
#10555=EDGE_CURVE('',#8121,#8120,#782,.T.);
#10556=EDGE_CURVE('',#8122,#8121,#783,.T.);
#10557=EDGE_CURVE('',#8122,#8123,#6471,.T.);
#10558=EDGE_CURVE('',#8124,#8123,#784,.F.);
#10559=EDGE_CURVE('',#8124,#8125,#4409,.T.);
#10560=EDGE_CURVE('',#8125,#8125,#6472,.T.);
#10561=EDGE_CURVE('',#8126,#8124,#785,.F.);
#10562=EDGE_CURVE('',#8127,#8126,#786,.T.);
#10563=EDGE_CURVE('',#8127,#8128,#6473,.T.);
#10564=EDGE_CURVE('',#8129,#8128,#787,.T.);
#10565=EDGE_CURVE('',#8130,#8129,#788,.T.);
#10566=EDGE_CURVE('',#8130,#8131,#6474,.T.);
#10567=EDGE_CURVE('',#8132,#8131,#789,.T.);
#10568=EDGE_CURVE('',#8133,#8132,#790,.T.);
#10569=EDGE_CURVE('',#8133,#8134,#6475,.T.);
#10570=EDGE_CURVE('',#8135,#8134,#791,.T.);
#10571=EDGE_CURVE('',#8136,#8135,#792,.T.);
#10572=EDGE_CURVE('',#8136,#8137,#6476,.T.);
#10573=EDGE_CURVE('',#8138,#8137,#793,.T.);
#10574=EDGE_CURVE('',#8139,#8138,#794,.T.);
#10575=EDGE_CURVE('',#8139,#8140,#6477,.T.);
#10576=EDGE_CURVE('',#8141,#8140,#795,.T.);
#10577=EDGE_CURVE('',#8142,#8141,#796,.T.);
#10578=EDGE_CURVE('',#8142,#8143,#6478,.T.);
#10579=EDGE_CURVE('',#8144,#8143,#797,.T.);
#10580=EDGE_CURVE('',#8145,#8144,#798,.T.);
#10581=EDGE_CURVE('',#8145,#8146,#6479,.T.);
#10582=EDGE_CURVE('',#8147,#8146,#799,.T.);
#10583=EDGE_CURVE('',#8148,#8147,#800,.T.);
#10584=EDGE_CURVE('',#8148,#8149,#6480,.T.);
#10585=EDGE_CURVE('',#8150,#8149,#801,.T.);
#10586=EDGE_CURVE('',#8151,#8150,#802,.T.);
#10587=EDGE_CURVE('',#8151,#8152,#6481,.T.);
#10588=EDGE_CURVE('',#8153,#8152,#803,.T.);
#10589=EDGE_CURVE('',#8154,#8153,#804,.T.);
#10590=EDGE_CURVE('',#8154,#8155,#6482,.T.);
#10591=EDGE_CURVE('',#8156,#8155,#805,.T.);
#10592=EDGE_CURVE('',#8157,#8156,#806,.T.);
#10593=EDGE_CURVE('',#8157,#8158,#6483,.T.);
#10594=EDGE_CURVE('',#8159,#8158,#807,.T.);
#10595=EDGE_CURVE('',#8160,#8159,#808,.T.);
#10596=EDGE_CURVE('',#8160,#8161,#6484,.T.);
#10597=EDGE_CURVE('',#8162,#8161,#809,.T.);
#10598=EDGE_CURVE('',#8163,#8162,#810,.T.);
#10599=EDGE_CURVE('',#8163,#8164,#6485,.T.);
#10600=EDGE_CURVE('',#8165,#8164,#811,.T.);
#10601=EDGE_CURVE('',#8166,#8165,#812,.T.);
#10602=EDGE_CURVE('',#8166,#8167,#6486,.T.);
#10603=EDGE_CURVE('',#8168,#8167,#813,.T.);
#10604=EDGE_CURVE('',#8169,#8168,#814,.T.);
#10605=EDGE_CURVE('',#8169,#8170,#6487,.T.);
#10606=EDGE_CURVE('',#8171,#8170,#815,.T.);
#10607=EDGE_CURVE('',#8172,#8171,#816,.T.);
#10608=EDGE_CURVE('',#8172,#8173,#6488,.T.);
#10609=EDGE_CURVE('',#8174,#8173,#817,.T.);
#10610=EDGE_CURVE('',#8175,#8174,#818,.T.);
#10611=EDGE_CURVE('',#8175,#8176,#6489,.T.);
#10612=EDGE_CURVE('',#8177,#8176,#819,.T.);
#10613=EDGE_CURVE('',#8178,#8177,#820,.T.);
#10614=EDGE_CURVE('',#8178,#8179,#6490,.T.);
#10615=EDGE_CURVE('',#8180,#8179,#821,.T.);
#10616=EDGE_CURVE('',#8181,#8180,#822,.T.);
#10617=EDGE_CURVE('',#8181,#8182,#6491,.T.);
#10618=EDGE_CURVE('',#8183,#8182,#823,.T.);
#10619=EDGE_CURVE('',#8184,#8183,#824,.T.);
#10620=EDGE_CURVE('',#8184,#8185,#6492,.T.);
#10621=EDGE_CURVE('',#8186,#8185,#825,.T.);
#10622=EDGE_CURVE('',#8187,#8186,#826,.T.);
#10623=EDGE_CURVE('',#8187,#8188,#6493,.T.);
#10624=EDGE_CURVE('',#8189,#8188,#827,.T.);
#10625=EDGE_CURVE('',#8190,#8189,#828,.T.);
#10626=EDGE_CURVE('',#8190,#8191,#6494,.T.);
#10627=EDGE_CURVE('',#8192,#8191,#829,.T.);
#10628=EDGE_CURVE('',#8193,#8192,#830,.T.);
#10629=EDGE_CURVE('',#8193,#8194,#6495,.T.);
#10630=EDGE_CURVE('',#8195,#8194,#831,.T.);
#10631=EDGE_CURVE('',#8196,#8195,#832,.T.);
#10632=EDGE_CURVE('',#8196,#8197,#6496,.T.);
#10633=EDGE_CURVE('',#8198,#8197,#833,.T.);
#10634=EDGE_CURVE('',#8199,#8198,#834,.T.);
#10635=EDGE_CURVE('',#8199,#8200,#6497,.T.);
#10636=EDGE_CURVE('',#8201,#8200,#835,.T.);
#10637=EDGE_CURVE('',#8202,#8201,#836,.T.);
#10638=EDGE_CURVE('',#8202,#8203,#6498,.T.);
#10639=EDGE_CURVE('',#8204,#8203,#837,.T.);
#10640=EDGE_CURVE('',#8205,#8204,#838,.T.);
#10641=EDGE_CURVE('',#8205,#8206,#6499,.T.);
#10642=EDGE_CURVE('',#8207,#8206,#839,.T.);
#10643=EDGE_CURVE('',#8208,#8207,#840,.T.);
#10644=EDGE_CURVE('',#8208,#8209,#6500,.T.);
#10645=EDGE_CURVE('',#8210,#8209,#841,.T.);
#10646=EDGE_CURVE('',#8211,#8210,#842,.T.);
#10647=EDGE_CURVE('',#8211,#8212,#6501,.T.);
#10648=EDGE_CURVE('',#8213,#8212,#843,.T.);
#10649=EDGE_CURVE('',#8214,#8213,#844,.T.);
#10650=EDGE_CURVE('',#8214,#8215,#6502,.T.);
#10651=EDGE_CURVE('',#8216,#8215,#845,.T.);
#10652=EDGE_CURVE('',#8217,#8216,#846,.T.);
#10653=EDGE_CURVE('',#8217,#8218,#6503,.T.);
#10654=EDGE_CURVE('',#8219,#8218,#847,.T.);
#10655=EDGE_CURVE('',#8220,#8219,#848,.T.);
#10656=EDGE_CURVE('',#8220,#8221,#6504,.T.);
#10657=EDGE_CURVE('',#8222,#8221,#849,.T.);
#10658=EDGE_CURVE('',#8223,#8222,#850,.T.);
#10659=EDGE_CURVE('',#8223,#8224,#6505,.T.);
#10660=EDGE_CURVE('',#8225,#8224,#851,.T.);
#10661=EDGE_CURVE('',#8226,#8225,#852,.T.);
#10662=EDGE_CURVE('',#8226,#8227,#6506,.T.);
#10663=EDGE_CURVE('',#8228,#8227,#853,.T.);
#10664=EDGE_CURVE('',#8229,#8228,#854,.T.);
#10665=EDGE_CURVE('',#8229,#8230,#6507,.T.);
#10666=EDGE_CURVE('',#8231,#8230,#855,.T.);
#10667=EDGE_CURVE('',#8232,#8231,#856,.T.);
#10668=EDGE_CURVE('',#8232,#8233,#6508,.T.);
#10669=EDGE_CURVE('',#8234,#8233,#857,.T.);
#10670=EDGE_CURVE('',#8235,#8234,#858,.T.);
#10671=EDGE_CURVE('',#8235,#8236,#6509,.T.);
#10672=EDGE_CURVE('',#8237,#8236,#859,.T.);
#10673=EDGE_CURVE('',#8238,#8237,#860,.T.);
#10674=EDGE_CURVE('',#8238,#8239,#6510,.T.);
#10675=EDGE_CURVE('',#8008,#8239,#861,.T.);
#10676=EDGE_CURVE('',#8240,#8240,#6511,.T.);
#10677=EDGE_CURVE('',#8240,#7769,#4410,.T.);
#10678=EDGE_CURVE('',#7955,#8178,#4411,.T.);
#10679=EDGE_CURVE('',#7954,#8179,#4412,.T.);
#10680=EDGE_CURVE('',#7957,#8176,#4413,.T.);
#10681=EDGE_CURVE('',#7958,#8175,#4414,.T.);
#10682=EDGE_CURVE('',#7960,#8173,#4415,.T.);
#10683=EDGE_CURVE('',#7961,#8172,#4416,.T.);
#10684=EDGE_CURVE('',#7963,#8170,#4417,.T.);
#10685=EDGE_CURVE('',#7964,#8169,#4418,.T.);
#10686=EDGE_CURVE('',#7966,#8167,#4419,.T.);
#10687=EDGE_CURVE('',#7967,#8166,#4420,.T.);
#10688=EDGE_CURVE('',#7969,#8164,#4421,.T.);
#10689=EDGE_CURVE('',#7970,#8163,#4422,.T.);
#10690=EDGE_CURVE('',#7972,#8161,#4423,.T.);
#10691=EDGE_CURVE('',#7973,#8160,#4424,.T.);
#10692=EDGE_CURVE('',#7975,#8158,#4425,.T.);
#10693=EDGE_CURVE('',#7976,#8157,#4426,.T.);
#10694=EDGE_CURVE('',#7978,#8155,#4427,.T.);
#10695=EDGE_CURVE('',#7979,#8154,#4428,.T.);
#10696=EDGE_CURVE('',#7981,#8152,#4429,.T.);
#10697=EDGE_CURVE('',#7982,#8151,#4430,.T.);
#10698=EDGE_CURVE('',#7984,#8149,#4431,.T.);
#10699=EDGE_CURVE('',#7985,#8148,#4432,.T.);
#10700=EDGE_CURVE('',#7987,#8146,#4433,.T.);
#10701=EDGE_CURVE('',#7988,#8145,#4434,.T.);
#10702=EDGE_CURVE('',#7990,#8143,#4435,.T.);
#10703=EDGE_CURVE('',#7991,#8142,#4436,.T.);
#10704=EDGE_CURVE('',#7993,#8140,#4437,.T.);
#10705=EDGE_CURVE('',#7994,#8139,#4438,.T.);
#10706=EDGE_CURVE('',#7996,#8137,#4439,.T.);
#10707=EDGE_CURVE('',#7997,#8136,#4440,.T.);
#10708=EDGE_CURVE('',#7999,#8134,#4441,.T.);
#10709=EDGE_CURVE('',#8000,#8133,#4442,.T.);
#10710=EDGE_CURVE('',#8002,#8131,#4443,.T.);
#10711=EDGE_CURVE('',#8003,#8130,#4444,.T.);
#10712=EDGE_CURVE('',#8005,#8128,#4445,.T.);
#10713=EDGE_CURVE('',#8006,#8127,#4446,.T.);
#10714=EDGE_CURVE('',#7775,#8123,#4447,.T.);
#10715=EDGE_CURVE('',#7776,#8122,#4448,.T.);
#10716=EDGE_CURVE('',#7778,#8120,#4449,.T.);
#10717=EDGE_CURVE('',#7779,#8119,#4450,.T.);
#10718=EDGE_CURVE('',#7781,#8117,#4451,.T.);
#10719=EDGE_CURVE('',#7782,#8116,#4452,.T.);
#10720=EDGE_CURVE('',#7784,#8114,#4453,.T.);
#10721=EDGE_CURVE('',#7785,#8113,#4454,.T.);
#10722=EDGE_CURVE('',#7787,#8111,#4455,.T.);
#10723=EDGE_CURVE('',#7788,#8110,#4456,.T.);
#10724=EDGE_CURVE('',#7790,#8108,#4457,.T.);
#10725=EDGE_CURVE('',#7791,#8107,#4458,.T.);
#10726=EDGE_CURVE('',#7793,#8105,#4459,.T.);
#10727=EDGE_CURVE('',#7794,#8104,#4460,.T.);
#10728=EDGE_CURVE('',#7796,#8102,#4461,.T.);
#10729=EDGE_CURVE('',#7797,#8101,#4462,.T.);
#10730=EDGE_CURVE('',#7799,#8099,#4463,.T.);
#10731=EDGE_CURVE('',#7800,#8098,#4464,.T.);
#10732=EDGE_CURVE('',#7802,#8096,#4465,.T.);
#10733=EDGE_CURVE('',#7803,#8095,#4466,.T.);
#10734=EDGE_CURVE('',#7805,#8093,#4467,.T.);
#10735=EDGE_CURVE('',#7806,#8092,#4468,.T.);
#10736=EDGE_CURVE('',#7808,#8090,#4469,.T.);
#10737=EDGE_CURVE('',#7809,#8089,#4470,.T.);
#10738=EDGE_CURVE('',#7811,#8087,#4471,.T.);
#10739=EDGE_CURVE('',#7812,#8086,#4472,.T.);
#10740=EDGE_CURVE('',#7814,#8084,#4473,.T.);
#10741=EDGE_CURVE('',#7815,#8083,#4474,.T.);
#10742=EDGE_CURVE('',#7817,#8081,#4475,.T.);
#10743=EDGE_CURVE('',#7818,#8080,#4476,.T.);
#10744=EDGE_CURVE('',#7820,#8078,#4477,.T.);
#10745=EDGE_CURVE('',#7821,#8077,#4478,.T.);
#10746=EDGE_CURVE('',#7823,#8075,#4479,.T.);
#10747=EDGE_CURVE('',#7824,#8074,#4480,.T.);
#10748=EDGE_CURVE('',#7826,#8072,#4481,.T.);
#10749=EDGE_CURVE('',#7827,#8071,#4482,.T.);
#10750=EDGE_CURVE('',#7829,#8069,#4483,.T.);
#10751=EDGE_CURVE('',#7830,#8068,#4484,.T.);
#10752=EDGE_CURVE('',#7832,#8066,#4485,.T.);
#10753=EDGE_CURVE('',#7833,#8065,#4486,.T.);
#10754=EDGE_CURVE('',#7835,#8063,#4487,.T.);
#10755=EDGE_CURVE('',#7836,#8062,#4488,.T.);
#10756=EDGE_CURVE('',#7838,#8060,#4489,.T.);
#10757=EDGE_CURVE('',#7839,#8059,#4490,.T.);
#10758=EDGE_CURVE('',#7841,#8057,#4491,.T.);
#10759=EDGE_CURVE('',#7842,#8056,#4492,.T.);
#10760=EDGE_CURVE('',#7844,#8054,#4493,.T.);
#10761=EDGE_CURVE('',#7845,#8053,#4494,.T.);
#10762=EDGE_CURVE('',#7847,#8051,#4495,.T.);
#10763=EDGE_CURVE('',#7848,#8050,#4496,.T.);
#10764=EDGE_CURVE('',#7850,#8048,#4497,.T.);
#10765=EDGE_CURVE('',#7851,#8047,#4498,.T.);
#10766=EDGE_CURVE('',#7853,#8045,#4499,.T.);
#10767=EDGE_CURVE('',#7854,#8044,#4500,.T.);
#10768=EDGE_CURVE('',#7856,#8042,#4501,.T.);
#10769=EDGE_CURVE('',#7857,#8041,#4502,.T.);
#10770=EDGE_CURVE('',#7859,#8039,#4503,.T.);
#10771=EDGE_CURVE('',#7860,#8038,#4504,.T.);
#10772=EDGE_CURVE('',#7862,#8036,#4505,.T.);
#10773=EDGE_CURVE('',#7863,#8035,#4506,.T.);
#10774=EDGE_CURVE('',#7865,#8033,#4507,.T.);
#10775=EDGE_CURVE('',#7866,#8032,#4508,.T.);
#10776=EDGE_CURVE('',#7868,#8030,#4509,.T.);
#10777=EDGE_CURVE('',#7869,#8029,#4510,.T.);
#10778=EDGE_CURVE('',#7871,#8027,#4511,.T.);
#10779=EDGE_CURVE('',#7872,#8026,#4512,.T.);
#10780=EDGE_CURVE('',#7874,#8024,#4513,.T.);
#10781=EDGE_CURVE('',#7875,#8023,#4514,.T.);
#10782=EDGE_CURVE('',#7877,#8021,#4515,.T.);
#10783=EDGE_CURVE('',#7878,#8020,#4516,.T.);
#10784=EDGE_CURVE('',#7880,#8018,#4517,.T.);
#10785=EDGE_CURVE('',#7881,#8017,#4518,.T.);
#10786=EDGE_CURVE('',#7883,#8015,#4519,.T.);
#10787=EDGE_CURVE('',#7884,#8014,#4520,.T.);
#10788=EDGE_CURVE('',#7886,#8012,#4521,.T.);
#10789=EDGE_CURVE('',#7887,#8011,#4522,.T.);
#10790=EDGE_CURVE('',#7889,#8009,#4523,.T.);
#10791=EDGE_CURVE('',#7890,#8007,#4524,.T.);
#10792=EDGE_CURVE('',#7894,#8239,#4525,.T.);
#10793=EDGE_CURVE('',#7895,#8238,#4526,.T.);
#10794=EDGE_CURVE('',#7897,#8236,#4527,.T.);
#10795=EDGE_CURVE('',#7898,#8235,#4528,.T.);
#10796=EDGE_CURVE('',#7900,#8233,#4529,.T.);
#10797=EDGE_CURVE('',#7901,#8232,#4530,.T.);
#10798=EDGE_CURVE('',#7903,#8230,#4531,.T.);
#10799=EDGE_CURVE('',#7904,#8229,#4532,.T.);
#10800=EDGE_CURVE('',#7906,#8227,#4533,.T.);
#10801=EDGE_CURVE('',#7907,#8226,#4534,.T.);
#10802=EDGE_CURVE('',#7909,#8224,#4535,.T.);
#10803=EDGE_CURVE('',#7910,#8223,#4536,.T.);
#10804=EDGE_CURVE('',#7912,#8221,#4537,.T.);
#10805=EDGE_CURVE('',#7913,#8220,#4538,.T.);
#10806=EDGE_CURVE('',#7915,#8218,#4539,.T.);
#10807=EDGE_CURVE('',#7916,#8217,#4540,.T.);
#10808=EDGE_CURVE('',#7918,#8215,#4541,.T.);
#10809=EDGE_CURVE('',#7919,#8214,#4542,.T.);
#10810=EDGE_CURVE('',#7921,#8212,#4543,.T.);
#10811=EDGE_CURVE('',#7922,#8211,#4544,.T.);
#10812=EDGE_CURVE('',#7924,#8209,#4545,.T.);
#10813=EDGE_CURVE('',#7925,#8208,#4546,.T.);
#10814=EDGE_CURVE('',#7927,#8206,#4547,.T.);
#10815=EDGE_CURVE('',#7928,#8205,#4548,.T.);
#10816=EDGE_CURVE('',#7930,#8203,#4549,.T.);
#10817=EDGE_CURVE('',#7931,#8202,#4550,.T.);
#10818=EDGE_CURVE('',#7933,#8200,#4551,.T.);
#10819=EDGE_CURVE('',#7934,#8199,#4552,.T.);
#10820=EDGE_CURVE('',#7936,#8197,#4553,.T.);
#10821=EDGE_CURVE('',#7937,#8196,#4554,.T.);
#10822=EDGE_CURVE('',#7939,#8194,#4555,.T.);
#10823=EDGE_CURVE('',#7940,#8193,#4556,.T.);
#10824=EDGE_CURVE('',#7942,#8191,#4557,.T.);
#10825=EDGE_CURVE('',#7943,#8190,#4558,.T.);
#10826=EDGE_CURVE('',#7945,#8188,#4559,.T.);
#10827=EDGE_CURVE('',#7946,#8187,#4560,.T.);
#10828=EDGE_CURVE('',#7952,#8181,#4561,.T.);
#10829=EDGE_CURVE('',#7951,#8182,#4562,.T.);
#10830=EDGE_CURVE('',#7948,#8185,#4563,.T.);
#10831=EDGE_CURVE('',#7949,#8184,#4564,.T.);
#10832=EDGE_CURVE('',#7950,#8183,#4565,.T.);
#10833=EDGE_CURVE('',#7953,#8180,#4566,.T.);
#10834=EDGE_CURVE('',#7947,#8186,#4567,.T.);
#10835=EDGE_CURVE('',#7944,#8189,#4568,.T.);
#10836=EDGE_CURVE('',#7941,#8192,#4569,.T.);
#10837=EDGE_CURVE('',#7938,#8195,#4570,.T.);
#10838=EDGE_CURVE('',#7935,#8198,#4571,.T.);
#10839=EDGE_CURVE('',#7932,#8201,#4572,.T.);
#10840=EDGE_CURVE('',#7929,#8204,#4573,.T.);
#10841=EDGE_CURVE('',#7926,#8207,#4574,.T.);
#10842=EDGE_CURVE('',#7923,#8210,#4575,.T.);
#10843=EDGE_CURVE('',#7920,#8213,#4576,.T.);
#10844=EDGE_CURVE('',#7917,#8216,#4577,.T.);
#10845=EDGE_CURVE('',#7914,#8219,#4578,.T.);
#10846=EDGE_CURVE('',#7911,#8222,#4579,.T.);
#10847=EDGE_CURVE('',#7908,#8225,#4580,.T.);
#10848=EDGE_CURVE('',#7905,#8228,#4581,.T.);
#10849=EDGE_CURVE('',#7902,#8231,#4582,.T.);
#10850=EDGE_CURVE('',#7899,#8234,#4583,.T.);
#10851=EDGE_CURVE('',#7896,#8237,#4584,.T.);
#10852=EDGE_CURVE('',#7893,#8008,#4585,.T.);
#10853=EDGE_CURVE('',#7888,#8010,#4586,.T.);
#10854=EDGE_CURVE('',#7885,#8013,#4587,.T.);
#10855=EDGE_CURVE('',#7882,#8016,#4588,.T.);
#10856=EDGE_CURVE('',#7879,#8019,#4589,.T.);
#10857=EDGE_CURVE('',#7876,#8022,#4590,.T.);
#10858=EDGE_CURVE('',#7873,#8025,#4591,.T.);
#10859=EDGE_CURVE('',#7870,#8028,#4592,.T.);
#10860=EDGE_CURVE('',#7867,#8031,#4593,.T.);
#10861=EDGE_CURVE('',#7864,#8034,#4594,.T.);
#10862=EDGE_CURVE('',#7861,#8037,#4595,.T.);
#10863=EDGE_CURVE('',#7858,#8040,#4596,.T.);
#10864=EDGE_CURVE('',#7855,#8043,#4597,.T.);
#10865=EDGE_CURVE('',#7852,#8046,#4598,.T.);
#10866=EDGE_CURVE('',#7849,#8049,#4599,.T.);
#10867=EDGE_CURVE('',#7846,#8052,#4600,.T.);
#10868=EDGE_CURVE('',#7843,#8055,#4601,.T.);
#10869=EDGE_CURVE('',#7840,#8058,#4602,.T.);
#10870=EDGE_CURVE('',#7837,#8061,#4603,.T.);
#10871=EDGE_CURVE('',#7834,#8064,#4604,.T.);
#10872=EDGE_CURVE('',#7831,#8067,#4605,.T.);
#10873=EDGE_CURVE('',#7828,#8070,#4606,.T.);
#10874=EDGE_CURVE('',#7825,#8073,#4607,.T.);
#10875=EDGE_CURVE('',#7822,#8076,#4608,.T.);
#10876=EDGE_CURVE('',#7819,#8079,#4609,.T.);
#10877=EDGE_CURVE('',#7816,#8082,#4610,.T.);
#10878=EDGE_CURVE('',#7813,#8085,#4611,.T.);
#10879=EDGE_CURVE('',#7810,#8088,#4612,.T.);
#10880=EDGE_CURVE('',#7807,#8091,#4613,.T.);
#10881=EDGE_CURVE('',#7804,#8094,#4614,.T.);
#10882=EDGE_CURVE('',#7801,#8097,#4615,.T.);
#10883=EDGE_CURVE('',#7798,#8100,#4616,.T.);
#10884=EDGE_CURVE('',#7795,#8103,#4617,.T.);
#10885=EDGE_CURVE('',#7792,#8106,#4618,.T.);
#10886=EDGE_CURVE('',#7789,#8109,#4619,.T.);
#10887=EDGE_CURVE('',#7786,#8112,#4620,.T.);
#10888=EDGE_CURVE('',#7783,#8115,#4621,.T.);
#10889=EDGE_CURVE('',#7780,#8118,#4622,.T.);
#10890=EDGE_CURVE('',#7777,#8121,#4623,.T.);
#10891=EDGE_CURVE('',#7774,#8126,#4624,.T.);
#10892=EDGE_CURVE('',#8004,#8129,#4625,.T.);
#10893=EDGE_CURVE('',#8001,#8132,#4626,.T.);
#10894=EDGE_CURVE('',#7998,#8135,#4627,.T.);
#10895=EDGE_CURVE('',#7995,#8138,#4628,.T.);
#10896=EDGE_CURVE('',#7992,#8141,#4629,.T.);
#10897=EDGE_CURVE('',#7989,#8144,#4630,.T.);
#10898=EDGE_CURVE('',#7986,#8147,#4631,.T.);
#10899=EDGE_CURVE('',#7983,#8150,#4632,.T.);
#10900=EDGE_CURVE('',#7980,#8153,#4633,.T.);
#10901=EDGE_CURVE('',#7977,#8156,#4634,.T.);
#10902=EDGE_CURVE('',#7974,#8159,#4635,.T.);
#10903=EDGE_CURVE('',#7971,#8162,#4636,.T.);
#10904=EDGE_CURVE('',#7968,#8165,#4637,.T.);
#10905=EDGE_CURVE('',#7965,#8168,#4638,.T.);
#10906=EDGE_CURVE('',#7962,#8171,#4639,.T.);
#10907=EDGE_CURVE('',#7959,#8174,#4640,.T.);
#10908=EDGE_CURVE('',#7956,#8177,#4641,.T.);
#10909=ORIENTED_EDGE('',*,*,#8241,.T.);
#10910=ORIENTED_EDGE('',*,*,#8242,.T.);
#10911=ORIENTED_EDGE('',*,*,#8243,.F.);
#10912=ORIENTED_EDGE('',*,*,#8244,.T.);
#10913=ORIENTED_EDGE('',*,*,#8245,.F.);
#10914=ORIENTED_EDGE('',*,*,#8246,.T.);
#10915=ORIENTED_EDGE('',*,*,#8247,.F.);
#10916=ORIENTED_EDGE('',*,*,#8248,.T.);
#10917=ORIENTED_EDGE('',*,*,#8249,.F.);
#10918=ORIENTED_EDGE('',*,*,#8250,.F.);
#10919=ORIENTED_EDGE('',*,*,#8251,.F.);
#10920=ORIENTED_EDGE('',*,*,#8252,.T.);
#10921=ORIENTED_EDGE('',*,*,#8253,.T.);
#10922=ORIENTED_EDGE('',*,*,#8242,.F.);
#10923=ORIENTED_EDGE('',*,*,#8254,.F.);
#10924=ORIENTED_EDGE('',*,*,#8246,.F.);
#10925=ORIENTED_EDGE('',*,*,#8255,.F.);
#10926=ORIENTED_EDGE('',*,*,#8248,.F.);
#10927=ORIENTED_EDGE('',*,*,#8256,.F.);
#10928=ORIENTED_EDGE('',*,*,#8244,.F.);
#10929=ORIENTED_EDGE('',*,*,#8257,.T.);
#10930=ORIENTED_EDGE('',*,*,#8258,.T.);
#10931=ORIENTED_EDGE('',*,*,#8259,.F.);
#10932=ORIENTED_EDGE('',*,*,#8260,.F.);
#10933=ORIENTED_EDGE('',*,*,#8261,.T.);
#10934=ORIENTED_EDGE('',*,*,#8259,.T.);
#10935=ORIENTED_EDGE('',*,*,#8262,.T.);
#10936=ORIENTED_EDGE('',*,*,#8251,.T.);
#10937=ORIENTED_EDGE('',*,*,#8257,.F.);
#10938=ORIENTED_EDGE('',*,*,#8243,.T.);
#10939=ORIENTED_EDGE('',*,*,#8253,.F.);
#10940=ORIENTED_EDGE('',*,*,#8263,.F.);
#10941=ORIENTED_EDGE('',*,*,#8258,.F.);
#10942=ORIENTED_EDGE('',*,*,#8263,.T.);
#10943=ORIENTED_EDGE('',*,*,#8252,.F.);
#10944=ORIENTED_EDGE('',*,*,#8262,.F.);
#10945=ORIENTED_EDGE('',*,*,#8254,.T.);
#10946=ORIENTED_EDGE('',*,*,#8241,.F.);
#10947=ORIENTED_EDGE('',*,*,#8256,.T.);
#10948=ORIENTED_EDGE('',*,*,#8247,.T.);
#10949=ORIENTED_EDGE('',*,*,#8249,.T.);
#10950=ORIENTED_EDGE('',*,*,#8245,.T.);
#10951=ORIENTED_EDGE('',*,*,#8255,.T.);
#10952=ORIENTED_EDGE('',*,*,#8264,.F.);
#10953=ORIENTED_EDGE('',*,*,#8250,.T.);
#10954=ORIENTED_EDGE('',*,*,#8264,.T.);
#10955=ORIENTED_EDGE('',*,*,#8260,.T.);
#10956=ORIENTED_EDGE('',*,*,#8261,.F.);
#10957=ORIENTED_EDGE('',*,*,#8265,.T.);
#10958=ORIENTED_EDGE('',*,*,#8266,.T.);
#10959=ORIENTED_EDGE('',*,*,#8267,.T.);
#10960=ORIENTED_EDGE('',*,*,#8268,.T.);
#10961=ORIENTED_EDGE('',*,*,#8269,.T.);
#10962=ORIENTED_EDGE('',*,*,#8270,.F.);
#10963=ORIENTED_EDGE('',*,*,#8271,.F.);
#10964=ORIENTED_EDGE('',*,*,#8272,.F.);
#10965=ORIENTED_EDGE('',*,*,#8273,.F.);
#10966=ORIENTED_EDGE('',*,*,#8274,.T.);
#10967=ORIENTED_EDGE('',*,*,#8275,.F.);
#10968=ORIENTED_EDGE('',*,*,#8276,.T.);
#10969=ORIENTED_EDGE('',*,*,#8277,.F.);
#10970=ORIENTED_EDGE('',*,*,#8268,.F.);
#10971=ORIENTED_EDGE('',*,*,#8278,.F.);
#10972=ORIENTED_EDGE('',*,*,#8270,.T.);
#10973=ORIENTED_EDGE('',*,*,#8279,.T.);
#10974=ORIENTED_EDGE('',*,*,#8280,.F.);
#10975=ORIENTED_EDGE('',*,*,#8281,.F.);
#10976=ORIENTED_EDGE('',*,*,#8276,.F.);
#10977=ORIENTED_EDGE('',*,*,#8282,.F.);
#10978=ORIENTED_EDGE('',*,*,#8274,.F.);
#10979=ORIENTED_EDGE('',*,*,#8283,.F.);
#10980=ORIENTED_EDGE('',*,*,#8284,.F.);
#10981=ORIENTED_EDGE('',*,*,#8285,.T.);
#10982=ORIENTED_EDGE('',*,*,#8272,.T.);
#10983=ORIENTED_EDGE('',*,*,#8286,.F.);
#10984=ORIENTED_EDGE('',*,*,#8266,.F.);
#10985=ORIENTED_EDGE('',*,*,#8267,.F.);
#10986=ORIENTED_EDGE('',*,*,#8286,.T.);
#10987=ORIENTED_EDGE('',*,*,#8271,.T.);
#10988=ORIENTED_EDGE('',*,*,#8278,.T.);
#10989=ORIENTED_EDGE('',*,*,#8285,.F.);
#10990=ORIENTED_EDGE('',*,*,#8287,.T.);
#10991=ORIENTED_EDGE('',*,*,#8279,.F.);
#10992=ORIENTED_EDGE('',*,*,#8269,.F.);
#10993=ORIENTED_EDGE('',*,*,#8281,.T.);
#10994=ORIENTED_EDGE('',*,*,#8288,.F.);
#10995=ORIENTED_EDGE('',*,*,#8283,.T.);
#10996=ORIENTED_EDGE('',*,*,#8273,.T.);
#10997=ORIENTED_EDGE('',*,*,#8280,.T.);
#10998=ORIENTED_EDGE('',*,*,#8287,.F.);
#10999=ORIENTED_EDGE('',*,*,#8284,.T.);
#11000=ORIENTED_EDGE('',*,*,#8288,.T.);
#11001=ORIENTED_EDGE('',*,*,#8277,.T.);
#11002=ORIENTED_EDGE('',*,*,#8275,.T.);
#11003=ORIENTED_EDGE('',*,*,#8282,.T.);
#11004=ORIENTED_EDGE('',*,*,#8265,.F.);
#11005=ORIENTED_EDGE('',*,*,#8289,.F.);
#11006=ORIENTED_EDGE('',*,*,#8290,.T.);
#11007=ORIENTED_EDGE('',*,*,#8291,.T.);
#11008=ORIENTED_EDGE('',*,*,#8292,.T.);
#11009=ORIENTED_EDGE('',*,*,#8293,.T.);
#11010=ORIENTED_EDGE('',*,*,#8294,.T.);
#11011=ORIENTED_EDGE('',*,*,#8289,.T.);
#11012=ORIENTED_EDGE('',*,*,#8295,.T.);
#11013=ORIENTED_EDGE('',*,*,#8296,.T.);
#11014=ORIENTED_EDGE('',*,*,#8297,.F.);
#11015=ORIENTED_EDGE('',*,*,#8298,.F.);
#11016=ORIENTED_EDGE('',*,*,#8299,.T.);
#11017=ORIENTED_EDGE('',*,*,#8291,.F.);
#11018=ORIENTED_EDGE('',*,*,#8300,.T.);
#11019=ORIENTED_EDGE('',*,*,#8301,.T.);
#11020=ORIENTED_EDGE('',*,*,#8302,.T.);
#11021=ORIENTED_EDGE('',*,*,#8303,.T.);
#11022=ORIENTED_EDGE('',*,*,#8304,.F.);
#11023=ORIENTED_EDGE('',*,*,#8305,.T.);
#11024=ORIENTED_EDGE('',*,*,#8306,.T.);
#11025=ORIENTED_EDGE('',*,*,#8307,.T.);
#11026=ORIENTED_EDGE('',*,*,#8299,.F.);
#11027=ORIENTED_EDGE('',*,*,#8308,.F.);
#11028=ORIENTED_EDGE('',*,*,#8302,.F.);
#11029=ORIENTED_EDGE('',*,*,#8297,.T.);
#11030=ORIENTED_EDGE('',*,*,#8309,.T.);
#11031=ORIENTED_EDGE('',*,*,#8304,.T.);
#11032=ORIENTED_EDGE('',*,*,#8310,.T.);
#11033=ORIENTED_EDGE('',*,*,#8310,.F.);
#11034=ORIENTED_EDGE('',*,*,#8303,.F.);
#11035=ORIENTED_EDGE('',*,*,#8308,.T.);
#11036=ORIENTED_EDGE('',*,*,#8298,.T.);
#11037=ORIENTED_EDGE('',*,*,#8292,.F.);
#11038=ORIENTED_EDGE('',*,*,#8306,.F.);
#11039=ORIENTED_EDGE('',*,*,#8311,.F.);
#11040=ORIENTED_EDGE('',*,*,#8295,.F.);
#11041=ORIENTED_EDGE('',*,*,#8311,.T.);
#11042=ORIENTED_EDGE('',*,*,#8305,.F.);
#11043=ORIENTED_EDGE('',*,*,#8309,.F.);
#11044=ORIENTED_EDGE('',*,*,#8296,.F.);
#11045=ORIENTED_EDGE('',*,*,#8312,.F.);
#11046=ORIENTED_EDGE('',*,*,#8300,.F.);
#11047=ORIENTED_EDGE('',*,*,#8290,.F.);
#11048=ORIENTED_EDGE('',*,*,#8294,.F.);
#11049=ORIENTED_EDGE('',*,*,#8307,.F.);
#11050=ORIENTED_EDGE('',*,*,#8301,.F.);
#11051=ORIENTED_EDGE('',*,*,#8312,.T.);
#11052=ORIENTED_EDGE('',*,*,#8293,.F.);
#11053=ORIENTED_EDGE('',*,*,#8313,.F.);
#11054=ORIENTED_EDGE('',*,*,#8314,.T.);
#11055=ORIENTED_EDGE('',*,*,#8315,.T.);
#11056=ORIENTED_EDGE('',*,*,#8316,.T.);
#11057=ORIENTED_EDGE('',*,*,#8317,.T.);
#11058=ORIENTED_EDGE('',*,*,#8318,.T.);
#11059=ORIENTED_EDGE('',*,*,#8313,.T.);
#11060=ORIENTED_EDGE('',*,*,#8319,.T.);
#11061=ORIENTED_EDGE('',*,*,#8320,.T.);
#11062=ORIENTED_EDGE('',*,*,#8321,.F.);
#11063=ORIENTED_EDGE('',*,*,#8322,.F.);
#11064=ORIENTED_EDGE('',*,*,#8323,.T.);
#11065=ORIENTED_EDGE('',*,*,#8315,.F.);
#11066=ORIENTED_EDGE('',*,*,#8324,.T.);
#11067=ORIENTED_EDGE('',*,*,#8325,.T.);
#11068=ORIENTED_EDGE('',*,*,#8326,.T.);
#11069=ORIENTED_EDGE('',*,*,#8327,.T.);
#11070=ORIENTED_EDGE('',*,*,#8328,.F.);
#11071=ORIENTED_EDGE('',*,*,#8329,.T.);
#11072=ORIENTED_EDGE('',*,*,#8330,.T.);
#11073=ORIENTED_EDGE('',*,*,#8331,.T.);
#11074=ORIENTED_EDGE('',*,*,#8323,.F.);
#11075=ORIENTED_EDGE('',*,*,#8332,.F.);
#11076=ORIENTED_EDGE('',*,*,#8326,.F.);
#11077=ORIENTED_EDGE('',*,*,#8321,.T.);
#11078=ORIENTED_EDGE('',*,*,#8333,.T.);
#11079=ORIENTED_EDGE('',*,*,#8328,.T.);
#11080=ORIENTED_EDGE('',*,*,#8334,.T.);
#11081=ORIENTED_EDGE('',*,*,#8334,.F.);
#11082=ORIENTED_EDGE('',*,*,#8327,.F.);
#11083=ORIENTED_EDGE('',*,*,#8332,.T.);
#11084=ORIENTED_EDGE('',*,*,#8322,.T.);
#11085=ORIENTED_EDGE('',*,*,#8316,.F.);
#11086=ORIENTED_EDGE('',*,*,#8330,.F.);
#11087=ORIENTED_EDGE('',*,*,#8335,.F.);
#11088=ORIENTED_EDGE('',*,*,#8319,.F.);
#11089=ORIENTED_EDGE('',*,*,#8335,.T.);
#11090=ORIENTED_EDGE('',*,*,#8329,.F.);
#11091=ORIENTED_EDGE('',*,*,#8333,.F.);
#11092=ORIENTED_EDGE('',*,*,#8320,.F.);
#11093=ORIENTED_EDGE('',*,*,#8336,.F.);
#11094=ORIENTED_EDGE('',*,*,#8324,.F.);
#11095=ORIENTED_EDGE('',*,*,#8314,.F.);
#11096=ORIENTED_EDGE('',*,*,#8318,.F.);
#11097=ORIENTED_EDGE('',*,*,#8331,.F.);
#11098=ORIENTED_EDGE('',*,*,#8325,.F.);
#11099=ORIENTED_EDGE('',*,*,#8336,.T.);
#11100=ORIENTED_EDGE('',*,*,#8317,.F.);
#11101=ORIENTED_EDGE('',*,*,#8337,.F.);
#11102=ORIENTED_EDGE('',*,*,#8338,.T.);
#11103=ORIENTED_EDGE('',*,*,#8339,.F.);
#11104=ORIENTED_EDGE('',*,*,#8340,.T.);
#11105=ORIENTED_EDGE('',*,*,#8341,.T.);
#11106=ORIENTED_EDGE('',*,*,#8342,.T.);
#11107=ORIENTED_EDGE('',*,*,#8343,.F.);
#11108=ORIENTED_EDGE('',*,*,#8340,.F.);
#11109=ORIENTED_EDGE('',*,*,#8344,.T.);
#11110=ORIENTED_EDGE('',*,*,#8338,.F.);
#11111=ORIENTED_EDGE('',*,*,#8345,.F.);
#11112=ORIENTED_EDGE('',*,*,#8346,.F.);
#11113=ORIENTED_EDGE('',*,*,#8342,.F.);
#11114=ORIENTED_EDGE('',*,*,#8347,.F.);
#11115=ORIENTED_EDGE('',*,*,#8344,.F.);
#11116=ORIENTED_EDGE('',*,*,#8339,.T.);
#11117=ORIENTED_EDGE('',*,*,#8343,.T.);
#11118=ORIENTED_EDGE('',*,*,#8348,.F.);
#11119=ORIENTED_EDGE('',*,*,#8345,.T.);
#11120=ORIENTED_EDGE('',*,*,#8337,.T.);
#11121=ORIENTED_EDGE('',*,*,#8347,.T.);
#11122=ORIENTED_EDGE('',*,*,#8341,.F.);
#11123=ORIENTED_EDGE('',*,*,#8346,.T.);
#11124=ORIENTED_EDGE('',*,*,#8348,.T.);
#11125=ORIENTED_EDGE('',*,*,#8349,.T.);
#11126=ORIENTED_EDGE('',*,*,#8350,.T.);
#11127=ORIENTED_EDGE('',*,*,#8351,.F.);
#11128=ORIENTED_EDGE('',*,*,#8352,.T.);
#11129=ORIENTED_EDGE('',*,*,#8353,.F.);
#11130=ORIENTED_EDGE('',*,*,#8354,.T.);
#11131=ORIENTED_EDGE('',*,*,#8355,.F.);
#11132=ORIENTED_EDGE('',*,*,#8356,.T.);
#11133=ORIENTED_EDGE('',*,*,#8351,.T.);
#11134=ORIENTED_EDGE('',*,*,#8357,.T.);
#11135=ORIENTED_EDGE('',*,*,#8358,.F.);
#11136=ORIENTED_EDGE('',*,*,#8354,.F.);
#11137=ORIENTED_EDGE('',*,*,#8359,.T.);
#11138=ORIENTED_EDGE('',*,*,#8356,.F.);
#11139=ORIENTED_EDGE('',*,*,#8360,.F.);
#11140=ORIENTED_EDGE('',*,*,#8352,.F.);
#11141=ORIENTED_EDGE('',*,*,#8357,.F.);
#11142=ORIENTED_EDGE('',*,*,#8350,.F.);
#11143=ORIENTED_EDGE('',*,*,#8359,.F.);
#11144=ORIENTED_EDGE('',*,*,#8353,.T.);
#11145=ORIENTED_EDGE('',*,*,#8358,.T.);
#11146=ORIENTED_EDGE('',*,*,#8349,.F.);
#11147=ORIENTED_EDGE('',*,*,#8360,.T.);
#11148=ORIENTED_EDGE('',*,*,#8355,.T.);
#11149=ORIENTED_EDGE('',*,*,#8361,.F.);
#11150=ORIENTED_EDGE('',*,*,#8362,.T.);
#11151=ORIENTED_EDGE('',*,*,#8363,.T.);
#11152=ORIENTED_EDGE('',*,*,#8364,.F.);
#11153=ORIENTED_EDGE('',*,*,#8365,.F.);
#11154=ORIENTED_EDGE('',*,*,#8366,.T.);
#11155=ORIENTED_EDGE('',*,*,#8367,.T.);
#11156=ORIENTED_EDGE('',*,*,#8368,.T.);
#11157=ORIENTED_EDGE('',*,*,#8369,.T.);
#11158=ORIENTED_EDGE('',*,*,#8370,.T.);
#11159=ORIENTED_EDGE('',*,*,#8361,.T.);
#11160=ORIENTED_EDGE('',*,*,#8371,.F.);
#11161=ORIENTED_EDGE('',*,*,#8372,.F.);
#11162=ORIENTED_EDGE('',*,*,#8373,.T.);
#11163=ORIENTED_EDGE('',*,*,#8365,.T.);
#11164=ORIENTED_EDGE('',*,*,#8374,.F.);
#11165=ORIENTED_EDGE('',*,*,#8363,.F.);
#11166=ORIENTED_EDGE('',*,*,#8375,.T.);
#11167=ORIENTED_EDGE('',*,*,#8376,.T.);
#11168=ORIENTED_EDGE('',*,*,#8377,.T.);
#11169=ORIENTED_EDGE('',*,*,#8378,.T.);
#11170=ORIENTED_EDGE('',*,*,#8379,.T.);
#11171=ORIENTED_EDGE('',*,*,#8372,.T.);
#11172=ORIENTED_EDGE('',*,*,#8380,.F.);
#11173=ORIENTED_EDGE('',*,*,#8377,.F.);
#11174=ORIENTED_EDGE('',*,*,#8381,.T.);
#11175=ORIENTED_EDGE('',*,*,#8368,.F.);
#11176=ORIENTED_EDGE('',*,*,#8382,.T.);
#11177=ORIENTED_EDGE('',*,*,#8364,.T.);
#11178=ORIENTED_EDGE('',*,*,#8380,.T.);
#11179=ORIENTED_EDGE('',*,*,#8374,.T.);
#11180=ORIENTED_EDGE('',*,*,#8371,.T.);
#11181=ORIENTED_EDGE('',*,*,#8383,.T.);
#11182=ORIENTED_EDGE('',*,*,#8378,.F.);
#11183=ORIENTED_EDGE('',*,*,#8382,.F.);
#11184=ORIENTED_EDGE('',*,*,#8367,.F.);
#11185=ORIENTED_EDGE('',*,*,#8373,.F.);
#11186=ORIENTED_EDGE('',*,*,#8379,.F.);
#11187=ORIENTED_EDGE('',*,*,#8383,.F.);
#11188=ORIENTED_EDGE('',*,*,#8366,.F.);
#11189=ORIENTED_EDGE('',*,*,#8384,.F.);
#11190=ORIENTED_EDGE('',*,*,#8375,.F.);
#11191=ORIENTED_EDGE('',*,*,#8362,.F.);
#11192=ORIENTED_EDGE('',*,*,#8370,.F.);
#11193=ORIENTED_EDGE('',*,*,#8381,.F.);
#11194=ORIENTED_EDGE('',*,*,#8376,.F.);
#11195=ORIENTED_EDGE('',*,*,#8384,.T.);
#11196=ORIENTED_EDGE('',*,*,#8369,.F.);
#11197=ORIENTED_EDGE('',*,*,#8385,.T.);
#11198=ORIENTED_EDGE('',*,*,#8386,.T.);
#11199=ORIENTED_EDGE('',*,*,#8385,.F.);
#11200=ORIENTED_EDGE('',*,*,#8386,.F.);
#11201=ORIENTED_EDGE('',*,*,#8387,.T.);
#11202=ORIENTED_EDGE('',*,*,#8388,.F.);
#11203=ORIENTED_EDGE('',*,*,#8387,.F.);
#11204=ORIENTED_EDGE('',*,*,#8389,.F.);
#11205=ORIENTED_EDGE('',*,*,#8390,.T.);
#11206=ORIENTED_EDGE('',*,*,#8391,.F.);
#11207=ORIENTED_EDGE('',*,*,#8390,.F.);
#11208=ORIENTED_EDGE('',*,*,#8392,.F.);
#11209=ORIENTED_EDGE('',*,*,#8393,.F.);
#11210=ORIENTED_EDGE('',*,*,#8394,.T.);
#11211=ORIENTED_EDGE('',*,*,#8395,.F.);
#11212=ORIENTED_EDGE('',*,*,#8394,.F.);
#11213=ORIENTED_EDGE('',*,*,#8396,.T.);
#11214=ORIENTED_EDGE('',*,*,#8397,.T.);
#11215=ORIENTED_EDGE('',*,*,#8389,.T.);
#11216=ORIENTED_EDGE('',*,*,#8397,.F.);
#11217=ORIENTED_EDGE('',*,*,#8388,.T.);
#11218=ORIENTED_EDGE('',*,*,#8398,.T.);
#11219=ORIENTED_EDGE('',*,*,#8399,.T.);
#11220=ORIENTED_EDGE('',*,*,#8392,.T.);
#11221=ORIENTED_EDGE('',*,*,#8393,.T.);
#11222=ORIENTED_EDGE('',*,*,#8399,.F.);
#11223=ORIENTED_EDGE('',*,*,#8395,.T.);
#11224=ORIENTED_EDGE('',*,*,#8396,.F.);
#11225=ORIENTED_EDGE('',*,*,#8398,.F.);
#11226=ORIENTED_EDGE('',*,*,#8391,.T.);
#11227=ORIENTED_EDGE('',*,*,#8400,.T.);
#11228=ORIENTED_EDGE('',*,*,#8401,.F.);
#11229=ORIENTED_EDGE('',*,*,#8402,.T.);
#11230=ORIENTED_EDGE('',*,*,#8403,.T.);
#11231=ORIENTED_EDGE('',*,*,#8404,.T.);
#11232=ORIENTED_EDGE('',*,*,#8405,.F.);
#11233=ORIENTED_EDGE('',*,*,#8400,.F.);
#11234=ORIENTED_EDGE('',*,*,#8406,.T.);
#11235=ORIENTED_EDGE('',*,*,#8407,.T.);
#11236=ORIENTED_EDGE('',*,*,#8408,.F.);
#11237=ORIENTED_EDGE('',*,*,#8404,.F.);
#11238=ORIENTED_EDGE('',*,*,#8409,.T.);
#11239=ORIENTED_EDGE('',*,*,#8410,.T.);
#11240=ORIENTED_EDGE('',*,*,#8411,.F.);
#11241=ORIENTED_EDGE('',*,*,#8407,.F.);
#11242=ORIENTED_EDGE('',*,*,#8412,.T.);
#11243=ORIENTED_EDGE('',*,*,#8413,.T.);
#11244=ORIENTED_EDGE('',*,*,#8414,.F.);
#11245=ORIENTED_EDGE('',*,*,#8410,.F.);
#11246=ORIENTED_EDGE('',*,*,#8415,.T.);
#11247=ORIENTED_EDGE('',*,*,#8416,.T.);
#11248=ORIENTED_EDGE('',*,*,#8417,.F.);
#11249=ORIENTED_EDGE('',*,*,#8413,.F.);
#11250=ORIENTED_EDGE('',*,*,#8418,.T.);
#11251=ORIENTED_EDGE('',*,*,#8419,.T.);
#11252=ORIENTED_EDGE('',*,*,#8420,.F.);
#11253=ORIENTED_EDGE('',*,*,#8416,.F.);
#11254=ORIENTED_EDGE('',*,*,#8421,.T.);
#11255=ORIENTED_EDGE('',*,*,#8422,.T.);
#11256=ORIENTED_EDGE('',*,*,#8423,.F.);
#11257=ORIENTED_EDGE('',*,*,#8419,.F.);
#11258=ORIENTED_EDGE('',*,*,#8424,.T.);
#11259=ORIENTED_EDGE('',*,*,#8425,.T.);
#11260=ORIENTED_EDGE('',*,*,#8426,.F.);
#11261=ORIENTED_EDGE('',*,*,#8422,.F.);
#11262=ORIENTED_EDGE('',*,*,#8427,.T.);
#11263=ORIENTED_EDGE('',*,*,#8428,.T.);
#11264=ORIENTED_EDGE('',*,*,#8429,.F.);
#11265=ORIENTED_EDGE('',*,*,#8425,.F.);
#11266=ORIENTED_EDGE('',*,*,#8430,.T.);
#11267=ORIENTED_EDGE('',*,*,#8431,.T.);
#11268=ORIENTED_EDGE('',*,*,#8432,.F.);
#11269=ORIENTED_EDGE('',*,*,#8428,.F.);
#11270=ORIENTED_EDGE('',*,*,#8433,.T.);
#11271=ORIENTED_EDGE('',*,*,#8434,.T.);
#11272=ORIENTED_EDGE('',*,*,#8435,.F.);
#11273=ORIENTED_EDGE('',*,*,#8431,.F.);
#11274=ORIENTED_EDGE('',*,*,#8436,.T.);
#11275=ORIENTED_EDGE('',*,*,#8437,.T.);
#11276=ORIENTED_EDGE('',*,*,#8438,.F.);
#11277=ORIENTED_EDGE('',*,*,#8434,.F.);
#11278=ORIENTED_EDGE('',*,*,#8439,.T.);
#11279=ORIENTED_EDGE('',*,*,#8440,.T.);
#11280=ORIENTED_EDGE('',*,*,#8441,.F.);
#11281=ORIENTED_EDGE('',*,*,#8437,.F.);
#11282=ORIENTED_EDGE('',*,*,#8442,.T.);
#11283=ORIENTED_EDGE('',*,*,#8443,.T.);
#11284=ORIENTED_EDGE('',*,*,#8444,.F.);
#11285=ORIENTED_EDGE('',*,*,#8440,.F.);
#11286=ORIENTED_EDGE('',*,*,#8445,.T.);
#11287=ORIENTED_EDGE('',*,*,#8446,.T.);
#11288=ORIENTED_EDGE('',*,*,#8447,.F.);
#11289=ORIENTED_EDGE('',*,*,#8443,.F.);
#11290=ORIENTED_EDGE('',*,*,#8448,.T.);
#11291=ORIENTED_EDGE('',*,*,#8449,.T.);
#11292=ORIENTED_EDGE('',*,*,#8450,.F.);
#11293=ORIENTED_EDGE('',*,*,#8446,.F.);
#11294=ORIENTED_EDGE('',*,*,#8451,.T.);
#11295=ORIENTED_EDGE('',*,*,#8452,.T.);
#11296=ORIENTED_EDGE('',*,*,#8453,.F.);
#11297=ORIENTED_EDGE('',*,*,#8449,.F.);
#11298=ORIENTED_EDGE('',*,*,#8454,.T.);
#11299=ORIENTED_EDGE('',*,*,#8455,.T.);
#11300=ORIENTED_EDGE('',*,*,#8456,.F.);
#11301=ORIENTED_EDGE('',*,*,#8452,.F.);
#11302=ORIENTED_EDGE('',*,*,#8457,.T.);
#11303=ORIENTED_EDGE('',*,*,#8458,.T.);
#11304=ORIENTED_EDGE('',*,*,#8459,.F.);
#11305=ORIENTED_EDGE('',*,*,#8455,.F.);
#11306=ORIENTED_EDGE('',*,*,#8460,.T.);
#11307=ORIENTED_EDGE('',*,*,#8461,.T.);
#11308=ORIENTED_EDGE('',*,*,#8462,.F.);
#11309=ORIENTED_EDGE('',*,*,#8458,.F.);
#11310=ORIENTED_EDGE('',*,*,#8463,.T.);
#11311=ORIENTED_EDGE('',*,*,#8464,.T.);
#11312=ORIENTED_EDGE('',*,*,#8465,.F.);
#11313=ORIENTED_EDGE('',*,*,#8461,.F.);
#11314=ORIENTED_EDGE('',*,*,#8466,.T.);
#11315=ORIENTED_EDGE('',*,*,#8467,.T.);
#11316=ORIENTED_EDGE('',*,*,#8468,.F.);
#11317=ORIENTED_EDGE('',*,*,#8464,.F.);
#11318=ORIENTED_EDGE('',*,*,#8469,.T.);
#11319=ORIENTED_EDGE('',*,*,#8470,.T.);
#11320=ORIENTED_EDGE('',*,*,#8471,.F.);
#11321=ORIENTED_EDGE('',*,*,#8467,.F.);
#11322=ORIENTED_EDGE('',*,*,#8472,.T.);
#11323=ORIENTED_EDGE('',*,*,#8473,.F.);
#11324=ORIENTED_EDGE('',*,*,#8474,.T.);
#11325=ORIENTED_EDGE('',*,*,#8475,.F.);
#11326=ORIENTED_EDGE('',*,*,#8476,.F.);
#11327=ORIENTED_EDGE('',*,*,#8477,.T.);
#11328=ORIENTED_EDGE('',*,*,#8478,.T.);
#11329=ORIENTED_EDGE('',*,*,#8479,.T.);
#11330=ORIENTED_EDGE('',*,*,#8480,.T.);
#11331=ORIENTED_EDGE('',*,*,#8481,.F.);
#11332=ORIENTED_EDGE('',*,*,#8482,.T.);
#11333=ORIENTED_EDGE('',*,*,#8483,.T.);
#11334=ORIENTED_EDGE('',*,*,#8477,.F.);
#11335=ORIENTED_EDGE('',*,*,#8484,.T.);
#11336=ORIENTED_EDGE('',*,*,#8485,.T.);
#11337=ORIENTED_EDGE('',*,*,#8486,.F.);
#11338=ORIENTED_EDGE('',*,*,#8480,.F.);
#11339=ORIENTED_EDGE('',*,*,#8487,.T.);
#11340=ORIENTED_EDGE('',*,*,#8488,.T.);
#11341=ORIENTED_EDGE('',*,*,#8489,.F.);
#11342=ORIENTED_EDGE('',*,*,#8485,.F.);
#11343=ORIENTED_EDGE('',*,*,#8490,.T.);
#11344=ORIENTED_EDGE('',*,*,#8491,.T.);
#11345=ORIENTED_EDGE('',*,*,#8492,.F.);
#11346=ORIENTED_EDGE('',*,*,#8488,.F.);
#11347=ORIENTED_EDGE('',*,*,#8493,.T.);
#11348=ORIENTED_EDGE('',*,*,#8494,.T.);
#11349=ORIENTED_EDGE('',*,*,#8495,.F.);
#11350=ORIENTED_EDGE('',*,*,#8491,.F.);
#11351=ORIENTED_EDGE('',*,*,#8496,.T.);
#11352=ORIENTED_EDGE('',*,*,#8497,.T.);
#11353=ORIENTED_EDGE('',*,*,#8498,.F.);
#11354=ORIENTED_EDGE('',*,*,#8494,.F.);
#11355=ORIENTED_EDGE('',*,*,#8499,.T.);
#11356=ORIENTED_EDGE('',*,*,#8500,.T.);
#11357=ORIENTED_EDGE('',*,*,#8501,.F.);
#11358=ORIENTED_EDGE('',*,*,#8497,.F.);
#11359=ORIENTED_EDGE('',*,*,#8502,.T.);
#11360=ORIENTED_EDGE('',*,*,#8503,.T.);
#11361=ORIENTED_EDGE('',*,*,#8504,.F.);
#11362=ORIENTED_EDGE('',*,*,#8500,.F.);
#11363=ORIENTED_EDGE('',*,*,#8505,.T.);
#11364=ORIENTED_EDGE('',*,*,#8506,.T.);
#11365=ORIENTED_EDGE('',*,*,#8507,.F.);
#11366=ORIENTED_EDGE('',*,*,#8503,.F.);
#11367=ORIENTED_EDGE('',*,*,#8508,.T.);
#11368=ORIENTED_EDGE('',*,*,#8509,.T.);
#11369=ORIENTED_EDGE('',*,*,#8510,.F.);
#11370=ORIENTED_EDGE('',*,*,#8506,.F.);
#11371=ORIENTED_EDGE('',*,*,#8511,.T.);
#11372=ORIENTED_EDGE('',*,*,#8512,.T.);
#11373=ORIENTED_EDGE('',*,*,#8513,.F.);
#11374=ORIENTED_EDGE('',*,*,#8509,.F.);
#11375=ORIENTED_EDGE('',*,*,#8514,.T.);
#11376=ORIENTED_EDGE('',*,*,#8515,.T.);
#11377=ORIENTED_EDGE('',*,*,#8516,.F.);
#11378=ORIENTED_EDGE('',*,*,#8512,.F.);
#11379=ORIENTED_EDGE('',*,*,#8517,.T.);
#11380=ORIENTED_EDGE('',*,*,#8518,.T.);
#11381=ORIENTED_EDGE('',*,*,#8519,.F.);
#11382=ORIENTED_EDGE('',*,*,#8515,.F.);
#11383=ORIENTED_EDGE('',*,*,#8520,.T.);
#11384=ORIENTED_EDGE('',*,*,#8521,.T.);
#11385=ORIENTED_EDGE('',*,*,#8522,.F.);
#11386=ORIENTED_EDGE('',*,*,#8518,.F.);
#11387=ORIENTED_EDGE('',*,*,#8523,.T.);
#11388=ORIENTED_EDGE('',*,*,#8524,.T.);
#11389=ORIENTED_EDGE('',*,*,#8525,.F.);
#11390=ORIENTED_EDGE('',*,*,#8521,.F.);
#11391=ORIENTED_EDGE('',*,*,#8526,.T.);
#11392=ORIENTED_EDGE('',*,*,#8527,.T.);
#11393=ORIENTED_EDGE('',*,*,#8528,.F.);
#11394=ORIENTED_EDGE('',*,*,#8524,.F.);
#11395=ORIENTED_EDGE('',*,*,#8529,.T.);
#11396=ORIENTED_EDGE('',*,*,#8530,.T.);
#11397=ORIENTED_EDGE('',*,*,#8531,.F.);
#11398=ORIENTED_EDGE('',*,*,#8527,.F.);
#11399=ORIENTED_EDGE('',*,*,#8532,.T.);
#11400=ORIENTED_EDGE('',*,*,#8533,.T.);
#11401=ORIENTED_EDGE('',*,*,#8534,.F.);
#11402=ORIENTED_EDGE('',*,*,#8530,.F.);
#11403=ORIENTED_EDGE('',*,*,#8535,.T.);
#11404=ORIENTED_EDGE('',*,*,#8536,.T.);
#11405=ORIENTED_EDGE('',*,*,#8537,.F.);
#11406=ORIENTED_EDGE('',*,*,#8533,.F.);
#11407=ORIENTED_EDGE('',*,*,#8538,.T.);
#11408=ORIENTED_EDGE('',*,*,#8539,.T.);
#11409=ORIENTED_EDGE('',*,*,#8540,.F.);
#11410=ORIENTED_EDGE('',*,*,#8536,.F.);
#11411=ORIENTED_EDGE('',*,*,#8541,.T.);
#11412=ORIENTED_EDGE('',*,*,#8542,.T.);
#11413=ORIENTED_EDGE('',*,*,#8543,.F.);
#11414=ORIENTED_EDGE('',*,*,#8539,.F.);
#11415=ORIENTED_EDGE('',*,*,#8544,.T.);
#11416=ORIENTED_EDGE('',*,*,#8545,.T.);
#11417=ORIENTED_EDGE('',*,*,#8546,.F.);
#11418=ORIENTED_EDGE('',*,*,#8542,.F.);
#11419=ORIENTED_EDGE('',*,*,#8547,.T.);
#11420=ORIENTED_EDGE('',*,*,#8548,.T.);
#11421=ORIENTED_EDGE('',*,*,#8549,.F.);
#11422=ORIENTED_EDGE('',*,*,#8545,.F.);
#11423=ORIENTED_EDGE('',*,*,#8550,.T.);
#11424=ORIENTED_EDGE('',*,*,#8551,.F.);
#11425=ORIENTED_EDGE('',*,*,#8552,.T.);
#11426=ORIENTED_EDGE('',*,*,#8553,.T.);
#11427=ORIENTED_EDGE('',*,*,#8554,.F.);
#11428=ORIENTED_EDGE('',*,*,#8483,.F.);
#11429=ORIENTED_EDGE('',*,*,#8478,.F.);
#11430=ORIENTED_EDGE('',*,*,#8555,.T.);
#11431=ORIENTED_EDGE('',*,*,#8556,.T.);
#11432=ORIENTED_EDGE('',*,*,#8555,.F.);
#11433=ORIENTED_EDGE('',*,*,#8557,.F.);
#11434=ORIENTED_EDGE('',*,*,#8558,.T.);
#11435=ORIENTED_EDGE('',*,*,#8559,.F.);
#11436=ORIENTED_EDGE('',*,*,#8560,.F.);
#11437=ORIENTED_EDGE('',*,*,#8561,.F.);
#11438=ORIENTED_EDGE('',*,*,#8562,.T.);
#11439=ORIENTED_EDGE('',*,*,#8563,.T.);
#11440=ORIENTED_EDGE('',*,*,#8562,.F.);
#11441=ORIENTED_EDGE('',*,*,#8564,.F.);
#11442=ORIENTED_EDGE('',*,*,#8565,.F.);
#11443=ORIENTED_EDGE('',*,*,#8566,.F.);
#11444=ORIENTED_EDGE('',*,*,#8558,.F.);
#11445=ORIENTED_EDGE('',*,*,#8567,.F.);
#11446=ORIENTED_EDGE('',*,*,#8568,.T.);
#11447=ORIENTED_EDGE('',*,*,#8569,.T.);
#11448=ORIENTED_EDGE('',*,*,#8568,.F.);
#11449=ORIENTED_EDGE('',*,*,#8570,.F.);
#11450=ORIENTED_EDGE('',*,*,#8571,.T.);
#11451=ORIENTED_EDGE('',*,*,#8572,.T.);
#11452=ORIENTED_EDGE('',*,*,#8573,.F.);
#11453=ORIENTED_EDGE('',*,*,#8574,.F.);
#11454=ORIENTED_EDGE('',*,*,#8575,.T.);
#11455=ORIENTED_EDGE('',*,*,#8567,.T.);
#11456=ORIENTED_EDGE('',*,*,#8575,.F.);
#11457=ORIENTED_EDGE('',*,*,#8576,.F.);
#11458=ORIENTED_EDGE('',*,*,#8577,.F.);
#11459=ORIENTED_EDGE('',*,*,#8578,.T.);
#11460=ORIENTED_EDGE('',*,*,#8571,.F.);
#11461=ORIENTED_EDGE('',*,*,#8579,.F.);
#11462=ORIENTED_EDGE('',*,*,#8580,.T.);
#11463=ORIENTED_EDGE('',*,*,#8581,.T.);
#11464=ORIENTED_EDGE('',*,*,#8580,.F.);
#11465=ORIENTED_EDGE('',*,*,#8582,.F.);
#11466=ORIENTED_EDGE('',*,*,#8583,.T.);
#11467=ORIENTED_EDGE('',*,*,#8579,.T.);
#11468=ORIENTED_EDGE('',*,*,#8583,.F.);
#11469=ORIENTED_EDGE('',*,*,#8584,.F.);
#11470=ORIENTED_EDGE('',*,*,#8585,.T.);
#11471=ORIENTED_EDGE('',*,*,#8586,.T.);
#11472=ORIENTED_EDGE('',*,*,#8585,.F.);
#11473=ORIENTED_EDGE('',*,*,#8551,.T.);
#11474=ORIENTED_EDGE('',*,*,#8587,.F.);
#11475=ORIENTED_EDGE('',*,*,#8548,.F.);
#11476=ORIENTED_EDGE('',*,*,#8588,.T.);
#11477=ORIENTED_EDGE('',*,*,#8557,.T.);
#11478=ORIENTED_EDGE('',*,*,#8553,.F.);
#11479=ORIENTED_EDGE('',*,*,#8589,.T.);
#11480=ORIENTED_EDGE('',*,*,#8475,.T.);
#11481=ORIENTED_EDGE('',*,*,#8590,.T.);
#11482=ORIENTED_EDGE('',*,*,#8584,.T.);
#11483=ORIENTED_EDGE('',*,*,#8563,.F.);
#11484=ORIENTED_EDGE('',*,*,#8582,.T.);
#11485=ORIENTED_EDGE('',*,*,#8586,.F.);
#11486=ORIENTED_EDGE('',*,*,#8581,.F.);
#11487=ORIENTED_EDGE('',*,*,#8570,.T.);
#11488=ORIENTED_EDGE('',*,*,#8569,.F.);
#11489=ORIENTED_EDGE('',*,*,#8556,.F.);
#11490=ORIENTED_EDGE('',*,*,#8565,.T.);
#11491=ORIENTED_EDGE('',*,*,#8591,.T.);
#11492=ORIENTED_EDGE('',*,*,#8577,.T.);
#11493=ORIENTED_EDGE('',*,*,#8592,.F.);
#11494=ORIENTED_EDGE('',*,*,#8559,.T.);
#11495=ORIENTED_EDGE('',*,*,#8566,.T.);
#11496=ORIENTED_EDGE('',*,*,#8592,.T.);
#11497=ORIENTED_EDGE('',*,*,#8576,.T.);
#11498=ORIENTED_EDGE('',*,*,#8574,.T.);
#11499=ORIENTED_EDGE('',*,*,#8593,.F.);
#11500=ORIENTED_EDGE('',*,*,#8560,.T.);
#11501=ORIENTED_EDGE('',*,*,#8593,.T.);
#11502=ORIENTED_EDGE('',*,*,#8573,.T.);
#11503=ORIENTED_EDGE('',*,*,#8594,.F.);
#11504=ORIENTED_EDGE('',*,*,#8564,.T.);
#11505=ORIENTED_EDGE('',*,*,#8561,.T.);
#11506=ORIENTED_EDGE('',*,*,#8594,.T.);
#11507=ORIENTED_EDGE('',*,*,#8572,.F.);
#11508=ORIENTED_EDGE('',*,*,#8578,.F.);
#11509=ORIENTED_EDGE('',*,*,#8591,.F.);
#11510=ORIENTED_EDGE('',*,*,#8402,.F.);
#11511=ORIENTED_EDGE('',*,*,#8595,.F.);
#11512=ORIENTED_EDGE('',*,*,#8482,.F.);
#11513=ORIENTED_EDGE('',*,*,#8596,.F.);
#11514=ORIENTED_EDGE('',*,*,#8473,.T.);
#11515=ORIENTED_EDGE('',*,*,#8597,.F.);
#11516=ORIENTED_EDGE('',*,*,#8470,.F.);
#11517=ORIENTED_EDGE('',*,*,#8598,.T.);
#11518=ORIENTED_EDGE('',*,*,#8479,.F.);
#11519=ORIENTED_EDGE('',*,*,#8595,.T.);
#11520=ORIENTED_EDGE('',*,*,#8401,.T.);
#11521=ORIENTED_EDGE('',*,*,#8405,.T.);
#11522=ORIENTED_EDGE('',*,*,#8408,.T.);
#11523=ORIENTED_EDGE('',*,*,#8411,.T.);
#11524=ORIENTED_EDGE('',*,*,#8414,.T.);
#11525=ORIENTED_EDGE('',*,*,#8417,.T.);
#11526=ORIENTED_EDGE('',*,*,#8420,.T.);
#11527=ORIENTED_EDGE('',*,*,#8423,.T.);
#11528=ORIENTED_EDGE('',*,*,#8426,.T.);
#11529=ORIENTED_EDGE('',*,*,#8429,.T.);
#11530=ORIENTED_EDGE('',*,*,#8432,.T.);
#11531=ORIENTED_EDGE('',*,*,#8435,.T.);
#11532=ORIENTED_EDGE('',*,*,#8438,.T.);
#11533=ORIENTED_EDGE('',*,*,#8441,.T.);
#11534=ORIENTED_EDGE('',*,*,#8444,.T.);
#11535=ORIENTED_EDGE('',*,*,#8447,.T.);
#11536=ORIENTED_EDGE('',*,*,#8450,.T.);
#11537=ORIENTED_EDGE('',*,*,#8453,.T.);
#11538=ORIENTED_EDGE('',*,*,#8456,.T.);
#11539=ORIENTED_EDGE('',*,*,#8459,.T.);
#11540=ORIENTED_EDGE('',*,*,#8462,.T.);
#11541=ORIENTED_EDGE('',*,*,#8465,.T.);
#11542=ORIENTED_EDGE('',*,*,#8468,.T.);
#11543=ORIENTED_EDGE('',*,*,#8471,.T.);
#11544=ORIENTED_EDGE('',*,*,#8597,.T.);
#11545=ORIENTED_EDGE('',*,*,#8476,.T.);
#11546=ORIENTED_EDGE('',*,*,#8589,.F.);
#11547=ORIENTED_EDGE('',*,*,#8552,.F.);
#11548=ORIENTED_EDGE('',*,*,#8588,.F.);
#11549=ORIENTED_EDGE('',*,*,#8550,.F.);
#11550=ORIENTED_EDGE('',*,*,#8547,.F.);
#11551=ORIENTED_EDGE('',*,*,#8544,.F.);
#11552=ORIENTED_EDGE('',*,*,#8541,.F.);
#11553=ORIENTED_EDGE('',*,*,#8538,.F.);
#11554=ORIENTED_EDGE('',*,*,#8535,.F.);
#11555=ORIENTED_EDGE('',*,*,#8532,.F.);
#11556=ORIENTED_EDGE('',*,*,#8529,.F.);
#11557=ORIENTED_EDGE('',*,*,#8526,.F.);
#11558=ORIENTED_EDGE('',*,*,#8523,.F.);
#11559=ORIENTED_EDGE('',*,*,#8520,.F.);
#11560=ORIENTED_EDGE('',*,*,#8517,.F.);
#11561=ORIENTED_EDGE('',*,*,#8514,.F.);
#11562=ORIENTED_EDGE('',*,*,#8511,.F.);
#11563=ORIENTED_EDGE('',*,*,#8508,.F.);
#11564=ORIENTED_EDGE('',*,*,#8505,.F.);
#11565=ORIENTED_EDGE('',*,*,#8502,.F.);
#11566=ORIENTED_EDGE('',*,*,#8499,.F.);
#11567=ORIENTED_EDGE('',*,*,#8496,.F.);
#11568=ORIENTED_EDGE('',*,*,#8493,.F.);
#11569=ORIENTED_EDGE('',*,*,#8490,.F.);
#11570=ORIENTED_EDGE('',*,*,#8487,.F.);
#11571=ORIENTED_EDGE('',*,*,#8484,.F.);
#11572=ORIENTED_EDGE('',*,*,#8403,.F.);
#11573=ORIENTED_EDGE('',*,*,#8596,.T.);
#11574=ORIENTED_EDGE('',*,*,#8481,.T.);
#11575=ORIENTED_EDGE('',*,*,#8486,.T.);
#11576=ORIENTED_EDGE('',*,*,#8489,.T.);
#11577=ORIENTED_EDGE('',*,*,#8492,.T.);
#11578=ORIENTED_EDGE('',*,*,#8495,.T.);
#11579=ORIENTED_EDGE('',*,*,#8498,.T.);
#11580=ORIENTED_EDGE('',*,*,#8501,.T.);
#11581=ORIENTED_EDGE('',*,*,#8504,.T.);
#11582=ORIENTED_EDGE('',*,*,#8507,.T.);
#11583=ORIENTED_EDGE('',*,*,#8510,.T.);
#11584=ORIENTED_EDGE('',*,*,#8513,.T.);
#11585=ORIENTED_EDGE('',*,*,#8516,.T.);
#11586=ORIENTED_EDGE('',*,*,#8519,.T.);
#11587=ORIENTED_EDGE('',*,*,#8522,.T.);
#11588=ORIENTED_EDGE('',*,*,#8525,.T.);
#11589=ORIENTED_EDGE('',*,*,#8528,.T.);
#11590=ORIENTED_EDGE('',*,*,#8531,.T.);
#11591=ORIENTED_EDGE('',*,*,#8534,.T.);
#11592=ORIENTED_EDGE('',*,*,#8537,.T.);
#11593=ORIENTED_EDGE('',*,*,#8540,.T.);
#11594=ORIENTED_EDGE('',*,*,#8543,.T.);
#11595=ORIENTED_EDGE('',*,*,#8546,.T.);
#11596=ORIENTED_EDGE('',*,*,#8549,.T.);
#11597=ORIENTED_EDGE('',*,*,#8587,.T.);
#11598=ORIENTED_EDGE('',*,*,#8554,.T.);
#11599=ORIENTED_EDGE('',*,*,#8590,.F.);
#11600=ORIENTED_EDGE('',*,*,#8474,.F.);
#11601=ORIENTED_EDGE('',*,*,#8598,.F.);
#11602=ORIENTED_EDGE('',*,*,#8472,.F.);
#11603=ORIENTED_EDGE('',*,*,#8469,.F.);
#11604=ORIENTED_EDGE('',*,*,#8466,.F.);
#11605=ORIENTED_EDGE('',*,*,#8463,.F.);
#11606=ORIENTED_EDGE('',*,*,#8460,.F.);
#11607=ORIENTED_EDGE('',*,*,#8457,.F.);
#11608=ORIENTED_EDGE('',*,*,#8454,.F.);
#11609=ORIENTED_EDGE('',*,*,#8451,.F.);
#11610=ORIENTED_EDGE('',*,*,#8448,.F.);
#11611=ORIENTED_EDGE('',*,*,#8445,.F.);
#11612=ORIENTED_EDGE('',*,*,#8442,.F.);
#11613=ORIENTED_EDGE('',*,*,#8439,.F.);
#11614=ORIENTED_EDGE('',*,*,#8436,.F.);
#11615=ORIENTED_EDGE('',*,*,#8433,.F.);
#11616=ORIENTED_EDGE('',*,*,#8430,.F.);
#11617=ORIENTED_EDGE('',*,*,#8427,.F.);
#11618=ORIENTED_EDGE('',*,*,#8424,.F.);
#11619=ORIENTED_EDGE('',*,*,#8421,.F.);
#11620=ORIENTED_EDGE('',*,*,#8418,.F.);
#11621=ORIENTED_EDGE('',*,*,#8415,.F.);
#11622=ORIENTED_EDGE('',*,*,#8412,.F.);
#11623=ORIENTED_EDGE('',*,*,#8409,.F.);
#11624=ORIENTED_EDGE('',*,*,#8406,.F.);
#11625=ORIENTED_EDGE('',*,*,#8599,.T.);
#11626=ORIENTED_EDGE('',*,*,#8600,.T.);
#11627=ORIENTED_EDGE('',*,*,#8601,.T.);
#11628=ORIENTED_EDGE('',*,*,#8600,.F.);
#11629=ORIENTED_EDGE('',*,*,#8602,.T.);
#11630=ORIENTED_EDGE('',*,*,#8603,.T.);
#11631=ORIENTED_EDGE('',*,*,#8604,.F.);
#11632=ORIENTED_EDGE('',*,*,#8603,.F.);
#11633=ORIENTED_EDGE('',*,*,#8602,.F.);
#11634=ORIENTED_EDGE('',*,*,#8604,.T.);
#11635=ORIENTED_EDGE('',*,*,#8599,.F.);
#11636=ORIENTED_EDGE('',*,*,#8601,.F.);
#11637=ORIENTED_EDGE('',*,*,#8605,.T.);
#11638=ORIENTED_EDGE('',*,*,#8606,.T.);
#11639=ORIENTED_EDGE('',*,*,#8607,.F.);
#11640=ORIENTED_EDGE('',*,*,#8606,.F.);
#11641=ORIENTED_EDGE('',*,*,#8608,.T.);
#11642=ORIENTED_EDGE('',*,*,#8609,.T.);
#11643=ORIENTED_EDGE('',*,*,#8610,.F.);
#11644=ORIENTED_EDGE('',*,*,#8609,.F.);
#11645=ORIENTED_EDGE('',*,*,#8610,.T.);
#11646=ORIENTED_EDGE('',*,*,#8605,.F.);
#11647=ORIENTED_EDGE('',*,*,#8608,.F.);
#11648=ORIENTED_EDGE('',*,*,#8607,.T.);
#11649=ORIENTED_EDGE('',*,*,#8611,.F.);
#11650=ORIENTED_EDGE('',*,*,#8612,.F.);
#11651=ORIENTED_EDGE('',*,*,#8613,.T.);
#11652=ORIENTED_EDGE('',*,*,#8614,.F.);
#11653=ORIENTED_EDGE('',*,*,#8613,.F.);
#11654=ORIENTED_EDGE('',*,*,#8615,.F.);
#11655=ORIENTED_EDGE('',*,*,#8616,.T.);
#11656=ORIENTED_EDGE('',*,*,#8617,.T.);
#11657=ORIENTED_EDGE('',*,*,#8616,.F.);
#11658=ORIENTED_EDGE('',*,*,#8617,.F.);
#11659=ORIENTED_EDGE('',*,*,#8618,.T.);
#11660=ORIENTED_EDGE('',*,*,#8619,.T.);
#11661=ORIENTED_EDGE('',*,*,#8618,.F.);
#11662=ORIENTED_EDGE('',*,*,#8611,.T.);
#11663=ORIENTED_EDGE('',*,*,#8612,.T.);
#11664=ORIENTED_EDGE('',*,*,#8620,.T.);
#11665=ORIENTED_EDGE('',*,*,#8615,.T.);
#11666=ORIENTED_EDGE('',*,*,#8620,.F.);
#11667=ORIENTED_EDGE('',*,*,#8614,.T.);
#11668=ORIENTED_EDGE('',*,*,#8619,.F.);
#11669=ORIENTED_EDGE('',*,*,#8621,.F.);
#11670=ORIENTED_EDGE('',*,*,#8622,.T.);
#11671=ORIENTED_EDGE('',*,*,#8623,.T.);
#11672=ORIENTED_EDGE('',*,*,#8622,.F.);
#11673=ORIENTED_EDGE('',*,*,#8623,.F.);
#11674=ORIENTED_EDGE('',*,*,#8624,.T.);
#11675=ORIENTED_EDGE('',*,*,#8625,.T.);
#11676=ORIENTED_EDGE('',*,*,#8624,.F.);
#11677=ORIENTED_EDGE('',*,*,#8625,.F.);
#11678=ORIENTED_EDGE('',*,*,#8626,.T.);
#11679=ORIENTED_EDGE('',*,*,#8627,.T.);
#11680=ORIENTED_EDGE('',*,*,#8626,.F.);
#11681=ORIENTED_EDGE('',*,*,#8628,.F.);
#11682=ORIENTED_EDGE('',*,*,#8629,.T.);
#11683=ORIENTED_EDGE('',*,*,#8630,.T.);
#11684=ORIENTED_EDGE('',*,*,#8629,.F.);
#11685=ORIENTED_EDGE('',*,*,#8630,.F.);
#11686=ORIENTED_EDGE('',*,*,#8631,.T.);
#11687=ORIENTED_EDGE('',*,*,#8632,.T.);
#11688=ORIENTED_EDGE('',*,*,#8631,.F.);
#11689=ORIENTED_EDGE('',*,*,#8633,.T.);
#11690=ORIENTED_EDGE('',*,*,#8633,.F.);
#11691=ORIENTED_EDGE('',*,*,#8634,.T.);
#11692=ORIENTED_EDGE('',*,*,#8634,.F.);
#11693=ORIENTED_EDGE('',*,*,#8635,.T.);
#11694=ORIENTED_EDGE('',*,*,#8636,.T.);
#11695=ORIENTED_EDGE('',*,*,#8635,.F.);
#11696=ORIENTED_EDGE('',*,*,#8621,.T.);
#11697=ORIENTED_EDGE('',*,*,#8636,.F.);
#11698=ORIENTED_EDGE('',*,*,#8632,.F.);
#11699=ORIENTED_EDGE('',*,*,#8627,.F.);
#11700=ORIENTED_EDGE('',*,*,#8628,.T.);
#11701=ORIENTED_EDGE('',*,*,#8637,.F.);
#11702=ORIENTED_EDGE('',*,*,#8638,.T.);
#11703=ORIENTED_EDGE('',*,*,#8639,.F.);
#11704=ORIENTED_EDGE('',*,*,#8638,.F.);
#11705=ORIENTED_EDGE('',*,*,#8640,.T.);
#11706=ORIENTED_EDGE('',*,*,#8641,.F.);
#11707=ORIENTED_EDGE('',*,*,#8642,.F.);
#11708=ORIENTED_EDGE('',*,*,#8643,.T.);
#11709=ORIENTED_EDGE('',*,*,#8644,.T.);
#11710=ORIENTED_EDGE('',*,*,#8645,.F.);
#11711=ORIENTED_EDGE('',*,*,#8642,.T.);
#11712=ORIENTED_EDGE('',*,*,#8643,.F.);
#11713=ORIENTED_EDGE('',*,*,#8646,.T.);
#11714=ORIENTED_EDGE('',*,*,#8647,.T.);
#11715=ORIENTED_EDGE('',*,*,#8648,.T.);
#11716=ORIENTED_EDGE('',*,*,#8649,.T.);
#11717=ORIENTED_EDGE('',*,*,#8650,.T.);
#11718=ORIENTED_EDGE('',*,*,#8651,.T.);
#11719=ORIENTED_EDGE('',*,*,#8652,.T.);
#11720=ORIENTED_EDGE('',*,*,#8648,.F.);
#11721=ORIENTED_EDGE('',*,*,#8653,.T.);
#11722=ORIENTED_EDGE('',*,*,#8654,.T.);
#11723=ORIENTED_EDGE('',*,*,#8651,.F.);
#11724=ORIENTED_EDGE('',*,*,#8655,.T.);
#11725=ORIENTED_EDGE('',*,*,#8656,.F.);
#11726=ORIENTED_EDGE('',*,*,#8656,.T.);
#11727=ORIENTED_EDGE('',*,*,#8657,.T.);
#11728=ORIENTED_EDGE('',*,*,#8658,.F.);
#11729=ORIENTED_EDGE('',*,*,#8659,.T.);
#11730=ORIENTED_EDGE('',*,*,#8660,.F.);
#11731=ORIENTED_EDGE('',*,*,#8661,.T.);
#11732=ORIENTED_EDGE('',*,*,#8662,.T.);
#11733=ORIENTED_EDGE('',*,*,#8663,.T.);
#11734=ORIENTED_EDGE('',*,*,#8664,.T.);
#11735=ORIENTED_EDGE('',*,*,#8637,.T.);
#11736=ORIENTED_EDGE('',*,*,#8664,.F.);
#11737=ORIENTED_EDGE('',*,*,#8665,.T.);
#11738=ORIENTED_EDGE('',*,*,#8666,.T.);
#11739=ORIENTED_EDGE('',*,*,#8667,.T.);
#11740=ORIENTED_EDGE('',*,*,#8645,.T.);
#11741=ORIENTED_EDGE('',*,*,#8668,.T.);
#11742=ORIENTED_EDGE('',*,*,#8669,.T.);
#11743=ORIENTED_EDGE('',*,*,#8665,.F.);
#11744=ORIENTED_EDGE('',*,*,#8663,.F.);
#11745=ORIENTED_EDGE('',*,*,#8670,.T.);
#11746=ORIENTED_EDGE('',*,*,#8671,.T.);
#11747=ORIENTED_EDGE('',*,*,#8659,.F.);
#11748=ORIENTED_EDGE('',*,*,#8672,.F.);
#11749=ORIENTED_EDGE('',*,*,#8673,.T.);
#11750=ORIENTED_EDGE('',*,*,#8674,.T.);
#11751=ORIENTED_EDGE('',*,*,#8675,.T.);
#11752=ORIENTED_EDGE('',*,*,#8674,.F.);
#11753=ORIENTED_EDGE('',*,*,#8676,.T.);
#11754=ORIENTED_EDGE('',*,*,#8677,.F.);
#11755=ORIENTED_EDGE('',*,*,#8639,.T.);
#11756=ORIENTED_EDGE('',*,*,#8675,.F.);
#11757=ORIENTED_EDGE('',*,*,#8672,.T.);
#11758=ORIENTED_EDGE('',*,*,#8658,.T.);
#11759=ORIENTED_EDGE('',*,*,#8678,.F.);
#11760=ORIENTED_EDGE('',*,*,#8677,.T.);
#11761=ORIENTED_EDGE('',*,*,#8679,.F.);
#11762=ORIENTED_EDGE('',*,*,#8660,.T.);
#11763=ORIENTED_EDGE('',*,*,#8678,.T.);
#11764=ORIENTED_EDGE('',*,*,#8680,.T.);
#11765=ORIENTED_EDGE('',*,*,#8681,.T.);
#11766=ORIENTED_EDGE('',*,*,#8682,.T.);
#11767=ORIENTED_EDGE('',*,*,#8683,.F.);
#11768=ORIENTED_EDGE('',*,*,#8684,.T.);
#11769=ORIENTED_EDGE('',*,*,#8685,.T.);
#11770=ORIENTED_EDGE('',*,*,#8686,.T.);
#11771=ORIENTED_EDGE('',*,*,#8687,.T.);
#11772=ORIENTED_EDGE('',*,*,#8688,.T.);
#11773=ORIENTED_EDGE('',*,*,#8689,.T.);
#11774=ORIENTED_EDGE('',*,*,#8690,.T.);
#11775=ORIENTED_EDGE('',*,*,#8679,.T.);
#11776=ORIENTED_EDGE('',*,*,#8676,.F.);
#11777=ORIENTED_EDGE('',*,*,#8673,.F.);
#11778=ORIENTED_EDGE('',*,*,#8683,.T.);
#11779=ORIENTED_EDGE('',*,*,#8691,.T.);
#11780=ORIENTED_EDGE('',*,*,#8692,.F.);
#11781=ORIENTED_EDGE('',*,*,#8693,.T.);
#11782=ORIENTED_EDGE('',*,*,#8687,.F.);
#11783=ORIENTED_EDGE('',*,*,#8694,.T.);
#11784=ORIENTED_EDGE('',*,*,#8695,.T.);
#11785=ORIENTED_EDGE('',*,*,#8696,.T.);
#11786=ORIENTED_EDGE('',*,*,#8695,.F.);
#11787=ORIENTED_EDGE('',*,*,#8697,.T.);
#11788=ORIENTED_EDGE('',*,*,#8698,.T.);
#11789=ORIENTED_EDGE('',*,*,#8692,.T.);
#11790=ORIENTED_EDGE('',*,*,#8699,.T.);
#11791=ORIENTED_EDGE('',*,*,#8700,.T.);
#11792=ORIENTED_EDGE('',*,*,#8690,.F.);
#11793=ORIENTED_EDGE('',*,*,#8701,.F.);
#11794=ORIENTED_EDGE('',*,*,#8654,.F.);
#11795=ORIENTED_EDGE('',*,*,#8701,.T.);
#11796=ORIENTED_EDGE('',*,*,#8689,.F.);
#11797=ORIENTED_EDGE('',*,*,#8702,.F.);
#11798=ORIENTED_EDGE('',*,*,#8652,.F.);
#11799=ORIENTED_EDGE('',*,*,#8702,.T.);
#11800=ORIENTED_EDGE('',*,*,#8688,.F.);
#11801=ORIENTED_EDGE('',*,*,#8703,.F.);
#11802=ORIENTED_EDGE('',*,*,#8649,.F.);
#11803=ORIENTED_EDGE('',*,*,#8703,.T.);
#11804=ORIENTED_EDGE('',*,*,#8696,.F.);
#11805=ORIENTED_EDGE('',*,*,#8704,.F.);
#11806=ORIENTED_EDGE('',*,*,#8705,.F.);
#11807=ORIENTED_EDGE('',*,*,#8650,.F.);
#11808=ORIENTED_EDGE('',*,*,#8704,.T.);
#11809=ORIENTED_EDGE('',*,*,#8698,.F.);
#11810=ORIENTED_EDGE('',*,*,#8644,.F.);
#11811=ORIENTED_EDGE('',*,*,#8705,.T.);
#11812=ORIENTED_EDGE('',*,*,#8706,.F.);
#11813=ORIENTED_EDGE('',*,*,#8706,.T.);
#11814=ORIENTED_EDGE('',*,*,#8697,.F.);
#11815=ORIENTED_EDGE('',*,*,#8707,.F.);
#11816=ORIENTED_EDGE('',*,*,#8668,.F.);
#11817=ORIENTED_EDGE('',*,*,#8707,.T.);
#11818=ORIENTED_EDGE('',*,*,#8694,.F.);
#11819=ORIENTED_EDGE('',*,*,#8708,.F.);
#11820=ORIENTED_EDGE('',*,*,#8708,.T.);
#11821=ORIENTED_EDGE('',*,*,#8686,.F.);
#11822=ORIENTED_EDGE('',*,*,#8709,.F.);
#11823=ORIENTED_EDGE('',*,*,#8666,.F.);
#11824=ORIENTED_EDGE('',*,*,#8669,.F.);
#11825=ORIENTED_EDGE('',*,*,#8709,.T.);
#11826=ORIENTED_EDGE('',*,*,#8685,.F.);
#11827=ORIENTED_EDGE('',*,*,#8710,.F.);
#11828=ORIENTED_EDGE('',*,*,#8661,.F.);
#11829=ORIENTED_EDGE('',*,*,#8667,.F.);
#11830=ORIENTED_EDGE('',*,*,#8710,.T.);
#11831=ORIENTED_EDGE('',*,*,#8684,.F.);
#11832=ORIENTED_EDGE('',*,*,#8711,.F.);
#11833=ORIENTED_EDGE('',*,*,#8670,.F.);
#11834=ORIENTED_EDGE('',*,*,#8662,.F.);
#11835=ORIENTED_EDGE('',*,*,#8711,.T.);
#11836=ORIENTED_EDGE('',*,*,#8693,.F.);
#11837=ORIENTED_EDGE('',*,*,#8712,.F.);
#11838=ORIENTED_EDGE('',*,*,#8640,.F.);
#11839=ORIENTED_EDGE('',*,*,#8671,.F.);
#11840=ORIENTED_EDGE('',*,*,#8712,.T.);
#11841=ORIENTED_EDGE('',*,*,#8700,.F.);
#11842=ORIENTED_EDGE('',*,*,#8641,.T.);
#11843=ORIENTED_EDGE('',*,*,#8699,.F.);
#11844=ORIENTED_EDGE('',*,*,#8713,.F.);
#11845=ORIENTED_EDGE('',*,*,#8646,.F.);
#11846=ORIENTED_EDGE('',*,*,#8713,.T.);
#11847=ORIENTED_EDGE('',*,*,#8691,.F.);
#11848=ORIENTED_EDGE('',*,*,#8714,.F.);
#11849=ORIENTED_EDGE('',*,*,#8714,.T.);
#11850=ORIENTED_EDGE('',*,*,#8682,.F.);
#11851=ORIENTED_EDGE('',*,*,#8715,.F.);
#11852=ORIENTED_EDGE('',*,*,#8647,.F.);
#11853=ORIENTED_EDGE('',*,*,#8715,.T.);
#11854=ORIENTED_EDGE('',*,*,#8681,.F.);
#11855=ORIENTED_EDGE('',*,*,#8716,.F.);
#11856=ORIENTED_EDGE('',*,*,#8653,.F.);
#11857=ORIENTED_EDGE('',*,*,#8655,.F.);
#11858=ORIENTED_EDGE('',*,*,#8716,.T.);
#11859=ORIENTED_EDGE('',*,*,#8680,.F.);
#11860=ORIENTED_EDGE('',*,*,#8657,.F.);
#11861=ORIENTED_EDGE('',*,*,#8717,.F.);
#11862=ORIENTED_EDGE('',*,*,#8718,.T.);
#11863=ORIENTED_EDGE('',*,*,#8719,.T.);
#11864=ORIENTED_EDGE('',*,*,#8720,.T.);
#11865=ORIENTED_EDGE('',*,*,#8721,.F.);
#11866=ORIENTED_EDGE('',*,*,#8722,.T.);
#11867=ORIENTED_EDGE('',*,*,#8723,.T.);
#11868=ORIENTED_EDGE('',*,*,#8722,.F.);
#11869=ORIENTED_EDGE('',*,*,#8717,.T.);
#11870=ORIENTED_EDGE('',*,*,#8724,.T.);
#11871=ORIENTED_EDGE('',*,*,#8725,.T.);
#11872=ORIENTED_EDGE('',*,*,#8726,.T.);
#11873=ORIENTED_EDGE('',*,*,#8719,.F.);
#11874=ORIENTED_EDGE('',*,*,#8727,.T.);
#11875=ORIENTED_EDGE('',*,*,#8728,.T.);
#11876=ORIENTED_EDGE('',*,*,#8727,.F.);
#11877=ORIENTED_EDGE('',*,*,#8725,.F.);
#11878=ORIENTED_EDGE('',*,*,#8728,.F.);
#11879=ORIENTED_EDGE('',*,*,#8729,.T.);
#11880=ORIENTED_EDGE('',*,*,#8730,.T.);
#11881=ORIENTED_EDGE('',*,*,#8729,.F.);
#11882=ORIENTED_EDGE('',*,*,#8730,.F.);
#11883=ORIENTED_EDGE('',*,*,#8731,.T.);
#11884=ORIENTED_EDGE('',*,*,#8732,.T.);
#11885=ORIENTED_EDGE('',*,*,#8731,.F.);
#11886=ORIENTED_EDGE('',*,*,#8732,.F.);
#11887=ORIENTED_EDGE('',*,*,#8720,.F.);
#11888=ORIENTED_EDGE('',*,*,#8724,.F.);
#11889=ORIENTED_EDGE('',*,*,#8723,.F.);
#11890=ORIENTED_EDGE('',*,*,#8726,.F.);
#11891=ORIENTED_EDGE('',*,*,#8718,.F.);
#11892=ORIENTED_EDGE('',*,*,#8721,.T.);
#11893=ORIENTED_EDGE('',*,*,#8733,.F.);
#11894=ORIENTED_EDGE('',*,*,#8734,.F.);
#11895=ORIENTED_EDGE('',*,*,#8735,.F.);
#11896=ORIENTED_EDGE('',*,*,#8736,.F.);
#11897=ORIENTED_EDGE('',*,*,#8737,.F.);
#11898=ORIENTED_EDGE('',*,*,#8738,.F.);
#11899=ORIENTED_EDGE('',*,*,#8739,.T.);
#11900=ORIENTED_EDGE('',*,*,#8740,.T.);
#11901=ORIENTED_EDGE('',*,*,#8741,.T.);
#11902=ORIENTED_EDGE('',*,*,#8742,.T.);
#11903=ORIENTED_EDGE('',*,*,#8743,.F.);
#11904=ORIENTED_EDGE('',*,*,#8744,.T.);
#11905=ORIENTED_EDGE('',*,*,#8745,.F.);
#11906=ORIENTED_EDGE('',*,*,#8733,.T.);
#11907=ORIENTED_EDGE('',*,*,#8746,.T.);
#11908=ORIENTED_EDGE('',*,*,#8747,.F.);
#11909=ORIENTED_EDGE('',*,*,#8748,.T.);
#11910=ORIENTED_EDGE('',*,*,#8749,.F.);
#11911=ORIENTED_EDGE('',*,*,#8748,.F.);
#11912=ORIENTED_EDGE('',*,*,#8750,.T.);
#11913=ORIENTED_EDGE('',*,*,#8751,.T.);
#11914=ORIENTED_EDGE('',*,*,#8752,.F.);
#11915=ORIENTED_EDGE('',*,*,#8753,.T.);
#11916=ORIENTED_EDGE('',*,*,#8754,.T.);
#11917=ORIENTED_EDGE('',*,*,#8755,.T.);
#11918=ORIENTED_EDGE('',*,*,#8755,.F.);
#11919=ORIENTED_EDGE('',*,*,#8756,.T.);
#11920=ORIENTED_EDGE('',*,*,#8744,.F.);
#11921=ORIENTED_EDGE('',*,*,#8757,.T.);
#11922=ORIENTED_EDGE('',*,*,#8742,.F.);
#11923=ORIENTED_EDGE('',*,*,#8758,.T.);
#11924=ORIENTED_EDGE('',*,*,#8743,.T.);
#11925=ORIENTED_EDGE('',*,*,#8759,.T.);
#11926=ORIENTED_EDGE('',*,*,#8760,.T.);
#11927=ORIENTED_EDGE('',*,*,#8759,.F.);
#11928=ORIENTED_EDGE('',*,*,#8757,.F.);
#11929=ORIENTED_EDGE('',*,*,#8761,.T.);
#11930=ORIENTED_EDGE('',*,*,#8762,.T.);
#11931=ORIENTED_EDGE('',*,*,#8747,.T.);
#11932=ORIENTED_EDGE('',*,*,#8762,.F.);
#11933=ORIENTED_EDGE('',*,*,#8763,.T.);
#11934=ORIENTED_EDGE('',*,*,#8764,.T.);
#11935=ORIENTED_EDGE('',*,*,#8765,.T.);
#11936=ORIENTED_EDGE('',*,*,#8738,.T.);
#11937=ORIENTED_EDGE('',*,*,#8752,.T.);
#11938=ORIENTED_EDGE('',*,*,#8766,.T.);
#11939=ORIENTED_EDGE('',*,*,#8767,.T.);
#11940=ORIENTED_EDGE('',*,*,#8768,.F.);
#11941=ORIENTED_EDGE('',*,*,#8768,.T.);
#11942=ORIENTED_EDGE('',*,*,#8769,.T.);
#11943=ORIENTED_EDGE('',*,*,#8763,.F.);
#11944=ORIENTED_EDGE('',*,*,#8761,.F.);
#11945=ORIENTED_EDGE('',*,*,#8737,.T.);
#11946=ORIENTED_EDGE('',*,*,#8770,.T.);
#11947=ORIENTED_EDGE('',*,*,#8770,.F.);
#11948=ORIENTED_EDGE('',*,*,#8736,.T.);
#11949=ORIENTED_EDGE('',*,*,#8771,.T.);
#11950=ORIENTED_EDGE('',*,*,#8749,.T.);
#11951=ORIENTED_EDGE('',*,*,#8760,.F.);
#11952=ORIENTED_EDGE('',*,*,#8772,.T.);
#11953=ORIENTED_EDGE('',*,*,#8773,.T.);
#11954=ORIENTED_EDGE('',*,*,#8774,.T.);
#11955=ORIENTED_EDGE('',*,*,#8734,.T.);
#11956=ORIENTED_EDGE('',*,*,#8745,.T.);
#11957=ORIENTED_EDGE('',*,*,#8741,.F.);
#11958=ORIENTED_EDGE('',*,*,#8775,.T.);
#11959=ORIENTED_EDGE('',*,*,#8776,.T.);
#11960=ORIENTED_EDGE('',*,*,#8777,.T.);
#11961=ORIENTED_EDGE('',*,*,#8778,.T.);
#11962=ORIENTED_EDGE('',*,*,#8778,.F.);
#11963=ORIENTED_EDGE('',*,*,#8779,.T.);
#11964=ORIENTED_EDGE('',*,*,#8750,.F.);
#11965=ORIENTED_EDGE('',*,*,#8758,.F.);
#11966=ORIENTED_EDGE('',*,*,#8754,.F.);
#11967=ORIENTED_EDGE('',*,*,#8780,.T.);
#11968=ORIENTED_EDGE('',*,*,#8772,.F.);
#11969=ORIENTED_EDGE('',*,*,#8756,.F.);
#11970=ORIENTED_EDGE('',*,*,#8779,.F.);
#11971=ORIENTED_EDGE('',*,*,#8777,.F.);
#11972=ORIENTED_EDGE('',*,*,#8781,.F.);
#11973=ORIENTED_EDGE('',*,*,#8751,.F.);
#11974=ORIENTED_EDGE('',*,*,#8781,.T.);
#11975=ORIENTED_EDGE('',*,*,#8776,.F.);
#11976=ORIENTED_EDGE('',*,*,#8782,.F.);
#11977=ORIENTED_EDGE('',*,*,#8766,.F.);
#11978=ORIENTED_EDGE('',*,*,#8775,.F.);
#11979=ORIENTED_EDGE('',*,*,#8740,.F.);
#11980=ORIENTED_EDGE('',*,*,#8783,.F.);
#11981=ORIENTED_EDGE('',*,*,#8764,.F.);
#11982=ORIENTED_EDGE('',*,*,#8769,.F.);
#11983=ORIENTED_EDGE('',*,*,#8767,.F.);
#11984=ORIENTED_EDGE('',*,*,#8782,.T.);
#11985=ORIENTED_EDGE('',*,*,#8783,.T.);
#11986=ORIENTED_EDGE('',*,*,#8746,.F.);
#11987=ORIENTED_EDGE('',*,*,#8739,.F.);
#11988=ORIENTED_EDGE('',*,*,#8765,.F.);
#11989=ORIENTED_EDGE('',*,*,#8735,.T.);
#11990=ORIENTED_EDGE('',*,*,#8774,.F.);
#11991=ORIENTED_EDGE('',*,*,#8784,.F.);
#11992=ORIENTED_EDGE('',*,*,#8771,.F.);
#11993=ORIENTED_EDGE('',*,*,#8784,.T.);
#11994=ORIENTED_EDGE('',*,*,#8773,.F.);
#11995=ORIENTED_EDGE('',*,*,#8780,.F.);
#11996=ORIENTED_EDGE('',*,*,#8753,.F.);
#11997=ORIENTED_EDGE('',*,*,#8785,.F.);
#11998=ORIENTED_EDGE('',*,*,#8786,.T.);
#11999=ORIENTED_EDGE('',*,*,#8787,.T.);
#12000=ORIENTED_EDGE('',*,*,#8788,.T.);
#12001=ORIENTED_EDGE('',*,*,#8789,.F.);
#12002=ORIENTED_EDGE('',*,*,#8790,.T.);
#12003=ORIENTED_EDGE('',*,*,#8791,.T.);
#12004=ORIENTED_EDGE('',*,*,#8790,.F.);
#12005=ORIENTED_EDGE('',*,*,#8785,.T.);
#12006=ORIENTED_EDGE('',*,*,#8792,.T.);
#12007=ORIENTED_EDGE('',*,*,#8793,.T.);
#12008=ORIENTED_EDGE('',*,*,#8794,.T.);
#12009=ORIENTED_EDGE('',*,*,#8787,.F.);
#12010=ORIENTED_EDGE('',*,*,#8795,.T.);
#12011=ORIENTED_EDGE('',*,*,#8796,.T.);
#12012=ORIENTED_EDGE('',*,*,#8795,.F.);
#12013=ORIENTED_EDGE('',*,*,#8793,.F.);
#12014=ORIENTED_EDGE('',*,*,#8796,.F.);
#12015=ORIENTED_EDGE('',*,*,#8797,.T.);
#12016=ORIENTED_EDGE('',*,*,#8798,.T.);
#12017=ORIENTED_EDGE('',*,*,#8797,.F.);
#12018=ORIENTED_EDGE('',*,*,#8798,.F.);
#12019=ORIENTED_EDGE('',*,*,#8799,.T.);
#12020=ORIENTED_EDGE('',*,*,#8800,.T.);
#12021=ORIENTED_EDGE('',*,*,#8799,.F.);
#12022=ORIENTED_EDGE('',*,*,#8800,.F.);
#12023=ORIENTED_EDGE('',*,*,#8788,.F.);
#12024=ORIENTED_EDGE('',*,*,#8792,.F.);
#12025=ORIENTED_EDGE('',*,*,#8791,.F.);
#12026=ORIENTED_EDGE('',*,*,#8794,.F.);
#12027=ORIENTED_EDGE('',*,*,#8786,.F.);
#12028=ORIENTED_EDGE('',*,*,#8789,.T.);
#12029=ORIENTED_EDGE('',*,*,#8801,.F.);
#12030=ORIENTED_EDGE('',*,*,#8802,.F.);
#12031=ORIENTED_EDGE('',*,*,#8803,.T.);
#12032=ORIENTED_EDGE('',*,*,#8804,.F.);
#12033=ORIENTED_EDGE('',*,*,#8803,.F.);
#12034=ORIENTED_EDGE('',*,*,#8805,.F.);
#12035=ORIENTED_EDGE('',*,*,#8806,.T.);
#12036=ORIENTED_EDGE('',*,*,#8807,.T.);
#12037=ORIENTED_EDGE('',*,*,#8806,.F.);
#12038=ORIENTED_EDGE('',*,*,#8808,.F.);
#12039=ORIENTED_EDGE('',*,*,#8809,.F.);
#12040=ORIENTED_EDGE('',*,*,#8810,.T.);
#12041=ORIENTED_EDGE('',*,*,#8805,.T.);
#12042=ORIENTED_EDGE('',*,*,#8810,.F.);
#12043=ORIENTED_EDGE('',*,*,#8808,.T.);
#12044=ORIENTED_EDGE('',*,*,#8809,.T.);
#12045=ORIENTED_EDGE('',*,*,#8811,.T.);
#12046=ORIENTED_EDGE('',*,*,#8812,.F.);
#12047=ORIENTED_EDGE('',*,*,#8813,.F.);
#12048=ORIENTED_EDGE('',*,*,#8811,.F.);
#12049=ORIENTED_EDGE('',*,*,#8814,.F.);
#12050=ORIENTED_EDGE('',*,*,#8815,.T.);
#12051=ORIENTED_EDGE('',*,*,#8812,.T.);
#12052=ORIENTED_EDGE('',*,*,#8813,.T.);
#12053=ORIENTED_EDGE('',*,*,#8815,.F.);
#12054=ORIENTED_EDGE('',*,*,#8816,.F.);
#12055=ORIENTED_EDGE('',*,*,#8817,.T.);
#12056=ORIENTED_EDGE('',*,*,#8818,.T.);
#12057=ORIENTED_EDGE('',*,*,#8817,.F.);
#12058=ORIENTED_EDGE('',*,*,#8801,.T.);
#12059=ORIENTED_EDGE('',*,*,#8802,.T.);
#12060=ORIENTED_EDGE('',*,*,#8819,.T.);
#12061=ORIENTED_EDGE('',*,*,#8820,.T.);
#12062=ORIENTED_EDGE('',*,*,#8819,.F.);
#12063=ORIENTED_EDGE('',*,*,#8804,.T.);
#12064=ORIENTED_EDGE('',*,*,#8820,.F.);
#12065=ORIENTED_EDGE('',*,*,#8816,.T.);
#12066=ORIENTED_EDGE('',*,*,#8818,.F.);
#12067=ORIENTED_EDGE('',*,*,#8814,.T.);
#12068=ORIENTED_EDGE('',*,*,#8807,.F.);
#12069=ORIENTED_EDGE('',*,*,#8821,.F.);
#12070=ORIENTED_EDGE('',*,*,#8822,.F.);
#12071=ORIENTED_EDGE('',*,*,#8823,.F.);
#12072=ORIENTED_EDGE('',*,*,#8824,.F.);
#12073=ORIENTED_EDGE('',*,*,#8825,.F.);
#12074=ORIENTED_EDGE('',*,*,#8826,.F.);
#12075=ORIENTED_EDGE('',*,*,#8827,.T.);
#12076=ORIENTED_EDGE('',*,*,#8828,.F.);
#12077=ORIENTED_EDGE('',*,*,#8829,.F.);
#12078=ORIENTED_EDGE('',*,*,#8830,.F.);
#12079=ORIENTED_EDGE('',*,*,#8831,.F.);
#12080=ORIENTED_EDGE('',*,*,#8832,.F.);
#12081=ORIENTED_EDGE('',*,*,#8833,.F.);
#12082=ORIENTED_EDGE('',*,*,#8834,.T.);
#12083=ORIENTED_EDGE('',*,*,#8835,.F.);
#12084=ORIENTED_EDGE('',*,*,#8836,.T.);
#12085=ORIENTED_EDGE('',*,*,#8837,.T.);
#12086=ORIENTED_EDGE('',*,*,#8838,.F.);
#12087=ORIENTED_EDGE('',*,*,#8839,.T.);
#12088=ORIENTED_EDGE('',*,*,#8840,.F.);
#12089=ORIENTED_EDGE('',*,*,#8841,.F.);
#12090=ORIENTED_EDGE('',*,*,#8842,.F.);
#12091=ORIENTED_EDGE('',*,*,#8843,.F.);
#12092=ORIENTED_EDGE('',*,*,#8844,.T.);
#12093=ORIENTED_EDGE('',*,*,#8845,.T.);
#12094=ORIENTED_EDGE('',*,*,#8846,.F.);
#12095=ORIENTED_EDGE('',*,*,#8847,.T.);
#12096=ORIENTED_EDGE('',*,*,#8848,.F.);
#12097=ORIENTED_EDGE('',*,*,#8849,.F.);
#12098=ORIENTED_EDGE('',*,*,#8850,.F.);
#12099=ORIENTED_EDGE('',*,*,#8851,.F.);
#12100=ORIENTED_EDGE('',*,*,#8852,.T.);
#12101=ORIENTED_EDGE('',*,*,#8853,.F.);
#12102=ORIENTED_EDGE('',*,*,#8854,.T.);
#12103=ORIENTED_EDGE('',*,*,#8855,.F.);
#12104=ORIENTED_EDGE('',*,*,#8856,.F.);
#12105=ORIENTED_EDGE('',*,*,#8857,.F.);
#12106=ORIENTED_EDGE('',*,*,#8858,.F.);
#12107=ORIENTED_EDGE('',*,*,#8859,.F.);
#12108=ORIENTED_EDGE('',*,*,#8860,.F.);
#12109=ORIENTED_EDGE('',*,*,#8849,.T.);
#12110=ORIENTED_EDGE('',*,*,#8861,.T.);
#12111=ORIENTED_EDGE('',*,*,#8862,.T.);
#12112=ORIENTED_EDGE('',*,*,#8848,.T.);
#12113=ORIENTED_EDGE('',*,*,#8841,.T.);
#12114=ORIENTED_EDGE('',*,*,#8863,.T.);
#12115=ORIENTED_EDGE('',*,*,#8864,.T.);
#12116=ORIENTED_EDGE('',*,*,#8840,.T.);
#12117=ORIENTED_EDGE('',*,*,#8833,.T.);
#12118=ORIENTED_EDGE('',*,*,#8865,.T.);
#12119=ORIENTED_EDGE('',*,*,#8866,.T.);
#12120=ORIENTED_EDGE('',*,*,#8867,.T.);
#12121=ORIENTED_EDGE('',*,*,#8868,.F.);
#12122=ORIENTED_EDGE('',*,*,#8869,.T.);
#12123=ORIENTED_EDGE('',*,*,#8870,.T.);
#12124=ORIENTED_EDGE('',*,*,#8869,.F.);
#12125=ORIENTED_EDGE('',*,*,#8871,.F.);
#12126=ORIENTED_EDGE('',*,*,#8872,.T.);
#12127=ORIENTED_EDGE('',*,*,#8873,.T.);
#12128=ORIENTED_EDGE('',*,*,#8872,.F.);
#12129=ORIENTED_EDGE('',*,*,#8874,.T.);
#12130=ORIENTED_EDGE('',*,*,#8875,.T.);
#12131=ORIENTED_EDGE('',*,*,#8876,.T.);
#12132=ORIENTED_EDGE('',*,*,#8877,.T.);
#12133=ORIENTED_EDGE('',*,*,#8878,.T.);
#12134=ORIENTED_EDGE('',*,*,#8879,.T.);
#12135=ORIENTED_EDGE('',*,*,#8880,.T.);
#12136=ORIENTED_EDGE('',*,*,#8826,.T.);
#12137=ORIENTED_EDGE('',*,*,#8881,.T.);
#12138=ORIENTED_EDGE('',*,*,#8858,.T.);
#12139=ORIENTED_EDGE('',*,*,#8882,.T.);
#12140=ORIENTED_EDGE('',*,*,#8846,.T.);
#12141=ORIENTED_EDGE('',*,*,#8883,.T.);
#12142=ORIENTED_EDGE('',*,*,#8884,.T.);
#12143=ORIENTED_EDGE('',*,*,#8885,.T.);
#12144=ORIENTED_EDGE('',*,*,#8838,.T.);
#12145=ORIENTED_EDGE('',*,*,#8886,.T.);
#12146=ORIENTED_EDGE('',*,*,#8887,.T.);
#12147=ORIENTED_EDGE('',*,*,#8888,.T.);
#12148=ORIENTED_EDGE('',*,*,#8889,.T.);
#12149=ORIENTED_EDGE('',*,*,#8890,.F.);
#12150=ORIENTED_EDGE('',*,*,#8891,.T.);
#12151=ORIENTED_EDGE('',*,*,#8878,.F.);
#12152=ORIENTED_EDGE('',*,*,#8892,.T.);
#12153=ORIENTED_EDGE('',*,*,#8893,.F.);
#12154=ORIENTED_EDGE('',*,*,#8894,.T.);
#12155=ORIENTED_EDGE('',*,*,#8874,.F.);
#12156=ORIENTED_EDGE('',*,*,#8895,.T.);
#12157=ORIENTED_EDGE('',*,*,#8882,.F.);
#12158=ORIENTED_EDGE('',*,*,#8896,.T.);
#12159=ORIENTED_EDGE('',*,*,#8897,.F.);
#12160=ORIENTED_EDGE('',*,*,#8898,.T.);
#12161=ORIENTED_EDGE('',*,*,#8885,.F.);
#12162=ORIENTED_EDGE('',*,*,#8899,.T.);
#12163=ORIENTED_EDGE('',*,*,#8900,.F.);
#12164=ORIENTED_EDGE('',*,*,#8901,.T.);
#12165=ORIENTED_EDGE('',*,*,#8902,.F.);
#12166=ORIENTED_EDGE('',*,*,#8903,.T.);
#12167=ORIENTED_EDGE('',*,*,#8904,.F.);
#12168=ORIENTED_EDGE('',*,*,#8905,.T.);
#12169=ORIENTED_EDGE('',*,*,#8880,.F.);
#12170=ORIENTED_EDGE('',*,*,#8906,.T.);
#12171=ORIENTED_EDGE('',*,*,#8907,.F.);
#12172=ORIENTED_EDGE('',*,*,#8908,.T.);
#12173=ORIENTED_EDGE('',*,*,#8876,.F.);
#12174=ORIENTED_EDGE('',*,*,#8909,.T.);
#12175=ORIENTED_EDGE('',*,*,#8910,.F.);
#12176=ORIENTED_EDGE('',*,*,#8911,.T.);
#12177=ORIENTED_EDGE('',*,*,#8912,.F.);
#12178=ORIENTED_EDGE('',*,*,#8913,.T.);
#12179=ORIENTED_EDGE('',*,*,#8881,.F.);
#12180=ORIENTED_EDGE('',*,*,#8914,.T.);
#12181=ORIENTED_EDGE('',*,*,#8915,.F.);
#12182=ORIENTED_EDGE('',*,*,#8916,.T.);
#12183=ORIENTED_EDGE('',*,*,#8883,.F.);
#12184=ORIENTED_EDGE('',*,*,#8917,.T.);
#12185=ORIENTED_EDGE('',*,*,#8918,.F.);
#12186=ORIENTED_EDGE('',*,*,#8919,.T.);
#12187=ORIENTED_EDGE('',*,*,#8920,.F.);
#12188=ORIENTED_EDGE('',*,*,#8921,.T.);
#12189=ORIENTED_EDGE('',*,*,#8897,.T.);
#12190=ORIENTED_EDGE('',*,*,#8922,.T.);
#12191=ORIENTED_EDGE('',*,*,#8890,.T.);
#12192=ORIENTED_EDGE('',*,*,#8923,.T.);
#12193=ORIENTED_EDGE('',*,*,#8893,.T.);
#12194=ORIENTED_EDGE('',*,*,#8924,.T.);
#12195=ORIENTED_EDGE('',*,*,#8904,.T.);
#12196=ORIENTED_EDGE('',*,*,#8835,.T.);
#12197=ORIENTED_EDGE('',*,*,#8925,.T.);
#12198=ORIENTED_EDGE('',*,*,#8843,.T.);
#12199=ORIENTED_EDGE('',*,*,#8900,.T.);
#12200=ORIENTED_EDGE('',*,*,#8851,.T.);
#12201=ORIENTED_EDGE('',*,*,#8920,.T.);
#12202=ORIENTED_EDGE('',*,*,#8926,.T.);
#12203=ORIENTED_EDGE('',*,*,#8902,.T.);
#12204=ORIENTED_EDGE('',*,*,#8927,.T.);
#12205=ORIENTED_EDGE('',*,*,#8907,.T.);
#12206=ORIENTED_EDGE('',*,*,#8855,.T.);
#12207=ORIENTED_EDGE('',*,*,#8912,.T.);
#12208=ORIENTED_EDGE('',*,*,#8928,.T.);
#12209=ORIENTED_EDGE('',*,*,#8915,.T.);
#12210=ORIENTED_EDGE('',*,*,#8929,.T.);
#12211=ORIENTED_EDGE('',*,*,#8930,.T.);
#12212=ORIENTED_EDGE('',*,*,#8931,.T.);
#12213=ORIENTED_EDGE('',*,*,#8918,.T.);
#12214=ORIENTED_EDGE('',*,*,#8823,.T.);
#12215=ORIENTED_EDGE('',*,*,#8910,.T.);
#12216=ORIENTED_EDGE('',*,*,#8831,.T.);
#12217=ORIENTED_EDGE('',*,*,#8871,.T.);
#12218=ORIENTED_EDGE('',*,*,#8873,.F.);
#12219=ORIENTED_EDGE('',*,*,#8868,.T.);
#12220=ORIENTED_EDGE('',*,*,#8870,.F.);
#12221=ORIENTED_EDGE('',*,*,#8888,.F.);
#12222=ORIENTED_EDGE('',*,*,#8932,.T.);
#12223=ORIENTED_EDGE('',*,*,#8925,.F.);
#12224=ORIENTED_EDGE('',*,*,#8933,.T.);
#12225=ORIENTED_EDGE('',*,*,#8930,.F.);
#12226=ORIENTED_EDGE('',*,*,#8934,.T.);
#12227=ORIENTED_EDGE('',*,*,#8886,.F.);
#12228=ORIENTED_EDGE('',*,*,#8935,.T.);
#12229=ORIENTED_EDGE('',*,*,#8936,.T.);
#12230=ORIENTED_EDGE('',*,*,#8937,.T.);
#12231=ORIENTED_EDGE('',*,*,#8938,.T.);
#12232=ORIENTED_EDGE('',*,*,#8821,.T.);
#12233=ORIENTED_EDGE('',*,*,#8853,.T.);
#12234=ORIENTED_EDGE('',*,*,#8939,.T.);
#12235=ORIENTED_EDGE('',*,*,#8940,.T.);
#12236=ORIENTED_EDGE('',*,*,#8860,.T.);
#12237=ORIENTED_EDGE('',*,*,#8941,.T.);
#12238=ORIENTED_EDGE('',*,*,#8942,.T.);
#12239=ORIENTED_EDGE('',*,*,#8828,.T.);
#12240=ORIENTED_EDGE('',*,*,#8829,.T.);
#12241=ORIENTED_EDGE('',*,*,#8896,.F.);
#12242=ORIENTED_EDGE('',*,*,#8857,.T.);
#12243=ORIENTED_EDGE('',*,*,#8943,.F.);
#12244=ORIENTED_EDGE('',*,*,#8859,.T.);
#12245=ORIENTED_EDGE('',*,*,#8913,.F.);
#12246=ORIENTED_EDGE('',*,*,#8854,.F.);
#12247=ORIENTED_EDGE('',*,*,#8943,.T.);
#12248=ORIENTED_EDGE('',*,*,#8940,.F.);
#12249=ORIENTED_EDGE('',*,*,#8944,.F.);
#12250=ORIENTED_EDGE('',*,*,#8922,.F.);
#12251=ORIENTED_EDGE('',*,*,#8891,.F.);
#12252=ORIENTED_EDGE('',*,*,#8944,.T.);
#12253=ORIENTED_EDGE('',*,*,#8945,.F.);
#12254=ORIENTED_EDGE('',*,*,#8856,.T.);
#12255=ORIENTED_EDGE('',*,*,#8906,.F.);
#12256=ORIENTED_EDGE('',*,*,#8946,.F.);
#12257=ORIENTED_EDGE('',*,*,#8945,.T.);
#12258=ORIENTED_EDGE('',*,*,#8939,.F.);
#12259=ORIENTED_EDGE('',*,*,#8946,.T.);
#12260=ORIENTED_EDGE('',*,*,#8879,.F.);
#12261=ORIENTED_EDGE('',*,*,#8947,.F.);
#12262=ORIENTED_EDGE('',*,*,#8884,.F.);
#12263=ORIENTED_EDGE('',*,*,#8948,.F.);
#12264=ORIENTED_EDGE('',*,*,#8861,.F.);
#12265=ORIENTED_EDGE('',*,*,#8899,.F.);
#12266=ORIENTED_EDGE('',*,*,#8947,.T.);
#12267=ORIENTED_EDGE('',*,*,#8852,.F.);
#12268=ORIENTED_EDGE('',*,*,#8948,.T.);
#12269=ORIENTED_EDGE('',*,*,#8916,.F.);
#12270=ORIENTED_EDGE('',*,*,#8949,.F.);
#12271=ORIENTED_EDGE('',*,*,#8949,.T.);
#12272=ORIENTED_EDGE('',*,*,#8928,.F.);
#12273=ORIENTED_EDGE('',*,*,#8950,.F.);
#12274=ORIENTED_EDGE('',*,*,#8862,.F.);
#12275=ORIENTED_EDGE('',*,*,#8898,.F.);
#12276=ORIENTED_EDGE('',*,*,#8850,.T.);
#12277=ORIENTED_EDGE('',*,*,#8847,.F.);
#12278=ORIENTED_EDGE('',*,*,#8950,.T.);
#12279=ORIENTED_EDGE('',*,*,#8914,.F.);
#12280=ORIENTED_EDGE('',*,*,#8845,.F.);
#12281=ORIENTED_EDGE('',*,*,#8951,.F.);
#12282=ORIENTED_EDGE('',*,*,#8887,.F.);
#12283=ORIENTED_EDGE('',*,*,#8952,.F.);
#12284=ORIENTED_EDGE('',*,*,#8863,.F.);
#12285=ORIENTED_EDGE('',*,*,#8932,.F.);
#12286=ORIENTED_EDGE('',*,*,#8951,.T.);
#12287=ORIENTED_EDGE('',*,*,#8844,.F.);
#12288=ORIENTED_EDGE('',*,*,#8952,.T.);
#12289=ORIENTED_EDGE('',*,*,#8934,.F.);
#12290=ORIENTED_EDGE('',*,*,#8953,.F.);
#12291=ORIENTED_EDGE('',*,*,#8953,.T.);
#12292=ORIENTED_EDGE('',*,*,#8929,.F.);
#12293=ORIENTED_EDGE('',*,*,#8954,.F.);
#12294=ORIENTED_EDGE('',*,*,#8864,.F.);
#12295=ORIENTED_EDGE('',*,*,#8901,.F.);
#12296=ORIENTED_EDGE('',*,*,#8842,.T.);
#12297=ORIENTED_EDGE('',*,*,#8839,.F.);
#12298=ORIENTED_EDGE('',*,*,#8954,.T.);
#12299=ORIENTED_EDGE('',*,*,#8917,.F.);
#12300=ORIENTED_EDGE('',*,*,#8837,.F.);
#12301=ORIENTED_EDGE('',*,*,#8955,.F.);
#12302=ORIENTED_EDGE('',*,*,#8931,.F.);
#12303=ORIENTED_EDGE('',*,*,#8956,.F.);
#12304=ORIENTED_EDGE('',*,*,#8866,.F.);
#12305=ORIENTED_EDGE('',*,*,#8919,.F.);
#12306=ORIENTED_EDGE('',*,*,#8955,.T.);
#12307=ORIENTED_EDGE('',*,*,#8957,.F.);
#12308=ORIENTED_EDGE('',*,*,#8956,.T.);
#12309=ORIENTED_EDGE('',*,*,#8935,.F.);
#12310=ORIENTED_EDGE('',*,*,#8958,.F.);
#12311=ORIENTED_EDGE('',*,*,#8957,.T.);
#12312=ORIENTED_EDGE('',*,*,#8865,.F.);
#12313=ORIENTED_EDGE('',*,*,#8959,.F.);
#12314=ORIENTED_EDGE('',*,*,#8926,.F.);
#12315=ORIENTED_EDGE('',*,*,#8958,.T.);
#12316=ORIENTED_EDGE('',*,*,#8889,.F.);
#12317=ORIENTED_EDGE('',*,*,#8960,.F.);
#12318=ORIENTED_EDGE('',*,*,#8867,.F.);
#12319=ORIENTED_EDGE('',*,*,#8903,.F.);
#12320=ORIENTED_EDGE('',*,*,#8959,.T.);
#12321=ORIENTED_EDGE('',*,*,#8836,.F.);
#12322=ORIENTED_EDGE('',*,*,#8960,.T.);
#12323=ORIENTED_EDGE('',*,*,#8933,.F.);
#12324=ORIENTED_EDGE('',*,*,#8834,.F.);
#12325=ORIENTED_EDGE('',*,*,#8908,.F.);
#12326=ORIENTED_EDGE('',*,*,#8830,.T.);
#12327=ORIENTED_EDGE('',*,*,#8827,.F.);
#12328=ORIENTED_EDGE('',*,*,#8832,.T.);
#12329=ORIENTED_EDGE('',*,*,#8909,.F.);
#12330=ORIENTED_EDGE('',*,*,#8961,.F.);
#12331=ORIENTED_EDGE('',*,*,#8961,.T.);
#12332=ORIENTED_EDGE('',*,*,#8875,.F.);
#12333=ORIENTED_EDGE('',*,*,#8962,.F.);
#12334=ORIENTED_EDGE('',*,*,#8941,.F.);
#12335=ORIENTED_EDGE('',*,*,#8892,.F.);
#12336=ORIENTED_EDGE('',*,*,#8825,.T.);
#12337=ORIENTED_EDGE('',*,*,#8963,.F.);
#12338=ORIENTED_EDGE('',*,*,#8962,.T.);
#12339=ORIENTED_EDGE('',*,*,#8894,.F.);
#12340=ORIENTED_EDGE('',*,*,#8964,.F.);
#12341=ORIENTED_EDGE('',*,*,#8963,.T.);
#12342=ORIENTED_EDGE('',*,*,#8942,.F.);
#12343=ORIENTED_EDGE('',*,*,#8964,.T.);
#12344=ORIENTED_EDGE('',*,*,#8923,.F.);
#12345=ORIENTED_EDGE('',*,*,#8911,.F.);
#12346=ORIENTED_EDGE('',*,*,#8822,.T.);
#12347=ORIENTED_EDGE('',*,*,#8965,.F.);
#12348=ORIENTED_EDGE('',*,*,#8824,.T.);
#12349=ORIENTED_EDGE('',*,*,#8921,.F.);
#12350=ORIENTED_EDGE('',*,*,#8966,.F.);
#12351=ORIENTED_EDGE('',*,*,#8965,.T.);
#12352=ORIENTED_EDGE('',*,*,#8938,.F.);
#12353=ORIENTED_EDGE('',*,*,#8967,.F.);
#12354=ORIENTED_EDGE('',*,*,#8877,.F.);
#12355=ORIENTED_EDGE('',*,*,#8966,.T.);
#12356=ORIENTED_EDGE('',*,*,#8927,.F.);
#12357=ORIENTED_EDGE('',*,*,#8968,.F.);
#12358=ORIENTED_EDGE('',*,*,#8936,.F.);
#12359=ORIENTED_EDGE('',*,*,#8895,.F.);
#12360=ORIENTED_EDGE('',*,*,#8967,.T.);
#12361=ORIENTED_EDGE('',*,*,#8969,.F.);
#12362=ORIENTED_EDGE('',*,*,#8968,.T.);
#12363=ORIENTED_EDGE('',*,*,#8905,.F.);
#12364=ORIENTED_EDGE('',*,*,#8970,.F.);
#12365=ORIENTED_EDGE('',*,*,#8969,.T.);
#12366=ORIENTED_EDGE('',*,*,#8937,.F.);
#12367=ORIENTED_EDGE('',*,*,#8970,.T.);
#12368=ORIENTED_EDGE('',*,*,#8924,.F.);
#12369=ORIENTED_EDGE('',*,*,#8971,.F.);
#12370=ORIENTED_EDGE('',*,*,#8972,.T.);
#12371=ORIENTED_EDGE('',*,*,#8973,.F.);
#12372=ORIENTED_EDGE('',*,*,#8972,.F.);
#12373=ORIENTED_EDGE('',*,*,#8974,.F.);
#12374=ORIENTED_EDGE('',*,*,#8975,.F.);
#12375=ORIENTED_EDGE('',*,*,#8976,.T.);
#12376=ORIENTED_EDGE('',*,*,#8977,.F.);
#12377=ORIENTED_EDGE('',*,*,#8976,.F.);
#12378=ORIENTED_EDGE('',*,*,#8978,.F.);
#12379=ORIENTED_EDGE('',*,*,#8979,.F.);
#12380=ORIENTED_EDGE('',*,*,#8980,.T.);
#12381=ORIENTED_EDGE('',*,*,#8981,.F.);
#12382=ORIENTED_EDGE('',*,*,#8980,.F.);
#12383=ORIENTED_EDGE('',*,*,#8982,.F.);
#12384=ORIENTED_EDGE('',*,*,#8983,.T.);
#12385=ORIENTED_EDGE('',*,*,#8984,.F.);
#12386=ORIENTED_EDGE('',*,*,#8983,.F.);
#12387=ORIENTED_EDGE('',*,*,#8985,.F.);
#12388=ORIENTED_EDGE('',*,*,#8986,.F.);
#12389=ORIENTED_EDGE('',*,*,#8987,.F.);
#12390=ORIENTED_EDGE('',*,*,#8988,.F.);
#12391=ORIENTED_EDGE('',*,*,#8989,.F.);
#12392=ORIENTED_EDGE('',*,*,#8990,.F.);
#12393=ORIENTED_EDGE('',*,*,#8991,.T.);
#12394=ORIENTED_EDGE('',*,*,#8992,.F.);
#12395=ORIENTED_EDGE('',*,*,#8991,.F.);
#12396=ORIENTED_EDGE('',*,*,#8993,.F.);
#12397=ORIENTED_EDGE('',*,*,#8994,.F.);
#12398=ORIENTED_EDGE('',*,*,#8995,.T.);
#12399=ORIENTED_EDGE('',*,*,#8996,.F.);
#12400=ORIENTED_EDGE('',*,*,#8995,.F.);
#12401=ORIENTED_EDGE('',*,*,#8997,.F.);
#12402=ORIENTED_EDGE('',*,*,#8998,.T.);
#12403=ORIENTED_EDGE('',*,*,#8999,.F.);
#12404=ORIENTED_EDGE('',*,*,#8998,.F.);
#12405=ORIENTED_EDGE('',*,*,#9000,.F.);
#12406=ORIENTED_EDGE('',*,*,#9001,.T.);
#12407=ORIENTED_EDGE('',*,*,#9002,.F.);
#12408=ORIENTED_EDGE('',*,*,#9001,.F.);
#12409=ORIENTED_EDGE('',*,*,#9003,.F.);
#12410=ORIENTED_EDGE('',*,*,#9004,.F.);
#12411=ORIENTED_EDGE('',*,*,#9005,.F.);
#12412=ORIENTED_EDGE('',*,*,#9006,.F.);
#12413=ORIENTED_EDGE('',*,*,#8993,.T.);
#12414=ORIENTED_EDGE('',*,*,#8994,.T.);
#12415=ORIENTED_EDGE('',*,*,#9007,.T.);
#12416=ORIENTED_EDGE('',*,*,#9008,.F.);
#12417=ORIENTED_EDGE('',*,*,#9009,.F.);
#12418=ORIENTED_EDGE('',*,*,#9010,.F.);
#12419=ORIENTED_EDGE('',*,*,#9007,.F.);
#12420=ORIENTED_EDGE('',*,*,#9011,.F.);
#12421=ORIENTED_EDGE('',*,*,#9012,.T.);
#12422=ORIENTED_EDGE('',*,*,#8971,.T.);
#12423=ORIENTED_EDGE('',*,*,#9012,.F.);
#12424=ORIENTED_EDGE('',*,*,#8989,.T.);
#12425=ORIENTED_EDGE('',*,*,#8990,.T.);
#12426=ORIENTED_EDGE('',*,*,#9013,.T.);
#12427=ORIENTED_EDGE('',*,*,#8982,.T.);
#12428=ORIENTED_EDGE('',*,*,#9013,.F.);
#12429=ORIENTED_EDGE('',*,*,#8985,.T.);
#12430=ORIENTED_EDGE('',*,*,#9014,.T.);
#12431=ORIENTED_EDGE('',*,*,#9003,.T.);
#12432=ORIENTED_EDGE('',*,*,#9015,.F.);
#12433=ORIENTED_EDGE('',*,*,#9009,.T.);
#12434=ORIENTED_EDGE('',*,*,#9016,.F.);
#12435=ORIENTED_EDGE('',*,*,#8978,.T.);
#12436=ORIENTED_EDGE('',*,*,#8979,.T.);
#12437=ORIENTED_EDGE('',*,*,#9017,.T.);
#12438=ORIENTED_EDGE('',*,*,#8997,.T.);
#12439=ORIENTED_EDGE('',*,*,#9017,.F.);
#12440=ORIENTED_EDGE('',*,*,#8974,.T.);
#12441=ORIENTED_EDGE('',*,*,#8975,.T.);
#12442=ORIENTED_EDGE('',*,*,#9018,.T.);
#12443=ORIENTED_EDGE('',*,*,#9000,.T.);
#12444=ORIENTED_EDGE('',*,*,#9018,.F.);
#12445=ORIENTED_EDGE('',*,*,#9019,.F.);
#12446=ORIENTED_EDGE('',*,*,#9020,.T.);
#12447=ORIENTED_EDGE('',*,*,#9021,.T.);
#12448=ORIENTED_EDGE('',*,*,#9022,.F.);
#12449=ORIENTED_EDGE('',*,*,#9023,.T.);
#12450=ORIENTED_EDGE('',*,*,#9024,.T.);
#12451=ORIENTED_EDGE('',*,*,#9025,.T.);
#12452=ORIENTED_EDGE('',*,*,#9026,.T.);
#12453=ORIENTED_EDGE('',*,*,#9027,.F.);
#12454=ORIENTED_EDGE('',*,*,#9028,.T.);
#12455=ORIENTED_EDGE('',*,*,#9029,.F.);
#12456=ORIENTED_EDGE('',*,*,#9030,.F.);
#12457=ORIENTED_EDGE('',*,*,#9031,.F.);
#12458=ORIENTED_EDGE('',*,*,#9021,.F.);
#12459=ORIENTED_EDGE('',*,*,#9032,.T.);
#12460=ORIENTED_EDGE('',*,*,#9033,.T.);
#12461=ORIENTED_EDGE('',*,*,#9034,.T.);
#12462=ORIENTED_EDGE('',*,*,#9035,.F.);
#12463=ORIENTED_EDGE('',*,*,#9036,.F.);
#12464=ORIENTED_EDGE('',*,*,#9037,.F.);
#12465=ORIENTED_EDGE('',*,*,#9038,.F.);
#12466=ORIENTED_EDGE('',*,*,#9039,.T.);
#12467=ORIENTED_EDGE('',*,*,#9040,.F.);
#12468=ORIENTED_EDGE('',*,*,#9005,.T.);
#12469=ORIENTED_EDGE('',*,*,#9002,.T.);
#12470=ORIENTED_EDGE('',*,*,#8999,.T.);
#12471=ORIENTED_EDGE('',*,*,#9035,.T.);
#12472=ORIENTED_EDGE('',*,*,#9041,.T.);
#12473=ORIENTED_EDGE('',*,*,#9042,.F.);
#12474=ORIENTED_EDGE('',*,*,#9043,.T.);
#12475=ORIENTED_EDGE('',*,*,#9044,.T.);
#12476=ORIENTED_EDGE('',*,*,#8987,.T.);
#12477=ORIENTED_EDGE('',*,*,#9045,.T.);
#12478=ORIENTED_EDGE('',*,*,#9046,.T.);
#12479=ORIENTED_EDGE('',*,*,#9047,.T.);
#12480=ORIENTED_EDGE('',*,*,#9048,.T.);
#12481=ORIENTED_EDGE('',*,*,#9049,.T.);
#12482=ORIENTED_EDGE('',*,*,#9042,.T.);
#12483=ORIENTED_EDGE('',*,*,#9050,.T.);
#12484=ORIENTED_EDGE('',*,*,#9051,.T.);
#12485=ORIENTED_EDGE('',*,*,#9052,.T.);
#12486=ORIENTED_EDGE('',*,*,#9053,.T.);
#12487=ORIENTED_EDGE('',*,*,#9054,.T.);
#12488=ORIENTED_EDGE('',*,*,#9055,.T.);
#12489=ORIENTED_EDGE('',*,*,#9056,.T.);
#12490=ORIENTED_EDGE('',*,*,#9019,.T.);
#12491=ORIENTED_EDGE('',*,*,#9057,.T.);
#12492=ORIENTED_EDGE('',*,*,#9058,.T.);
#12493=ORIENTED_EDGE('',*,*,#9059,.T.);
#12494=ORIENTED_EDGE('',*,*,#9060,.T.);
#12495=ORIENTED_EDGE('',*,*,#9061,.T.);
#12496=ORIENTED_EDGE('',*,*,#9062,.T.);
#12497=ORIENTED_EDGE('',*,*,#9063,.T.);
#12498=ORIENTED_EDGE('',*,*,#9064,.F.);
#12499=ORIENTED_EDGE('',*,*,#9065,.T.);
#12500=ORIENTED_EDGE('',*,*,#9066,.T.);
#12501=ORIENTED_EDGE('',*,*,#9067,.T.);
#12502=ORIENTED_EDGE('',*,*,#9068,.T.);
#12503=ORIENTED_EDGE('',*,*,#9069,.F.);
#12504=ORIENTED_EDGE('',*,*,#9070,.F.);
#12505=ORIENTED_EDGE('',*,*,#9064,.T.);
#12506=ORIENTED_EDGE('',*,*,#9071,.T.);
#12507=ORIENTED_EDGE('',*,*,#8981,.T.);
#12508=ORIENTED_EDGE('',*,*,#8977,.T.);
#12509=ORIENTED_EDGE('',*,*,#9072,.T.);
#12510=ORIENTED_EDGE('',*,*,#9073,.T.);
#12511=ORIENTED_EDGE('',*,*,#9074,.T.);
#12512=ORIENTED_EDGE('',*,*,#9075,.T.);
#12513=ORIENTED_EDGE('',*,*,#9076,.T.);
#12514=ORIENTED_EDGE('',*,*,#9077,.T.);
#12515=ORIENTED_EDGE('',*,*,#9078,.T.);
#12516=ORIENTED_EDGE('',*,*,#8973,.T.);
#12517=ORIENTED_EDGE('',*,*,#9079,.T.);
#12518=ORIENTED_EDGE('',*,*,#9080,.T.);
#12519=ORIENTED_EDGE('',*,*,#9081,.T.);
#12520=ORIENTED_EDGE('',*,*,#9082,.T.);
#12521=ORIENTED_EDGE('',*,*,#9083,.T.);
#12522=ORIENTED_EDGE('',*,*,#9084,.T.);
#12523=ORIENTED_EDGE('',*,*,#9085,.T.);
#12524=ORIENTED_EDGE('',*,*,#9086,.T.);
#12525=ORIENTED_EDGE('',*,*,#9087,.T.);
#12526=ORIENTED_EDGE('',*,*,#8996,.T.);
#12527=ORIENTED_EDGE('',*,*,#9088,.T.);
#12528=ORIENTED_EDGE('',*,*,#9089,.T.);
#12529=ORIENTED_EDGE('',*,*,#9090,.F.);
#12530=ORIENTED_EDGE('',*,*,#9091,.T.);
#12531=ORIENTED_EDGE('',*,*,#9040,.T.);
#12532=ORIENTED_EDGE('',*,*,#9092,.T.);
#12533=ORIENTED_EDGE('',*,*,#9088,.F.);
#12534=ORIENTED_EDGE('',*,*,#9093,.T.);
#12535=ORIENTED_EDGE('',*,*,#9045,.F.);
#12536=ORIENTED_EDGE('',*,*,#8986,.T.);
#12537=ORIENTED_EDGE('',*,*,#9016,.T.);
#12538=ORIENTED_EDGE('',*,*,#9008,.T.);
#12539=ORIENTED_EDGE('',*,*,#9010,.T.);
#12540=ORIENTED_EDGE('',*,*,#9015,.T.);
#12541=ORIENTED_EDGE('',*,*,#9006,.T.);
#12542=ORIENTED_EDGE('',*,*,#9094,.T.);
#12543=ORIENTED_EDGE('',*,*,#9095,.T.);
#12544=ORIENTED_EDGE('',*,*,#9027,.T.);
#12545=ORIENTED_EDGE('',*,*,#9004,.T.);
#12546=ORIENTED_EDGE('',*,*,#9014,.F.);
#12547=ORIENTED_EDGE('',*,*,#8988,.T.);
#12548=ORIENTED_EDGE('',*,*,#9044,.F.);
#12549=ORIENTED_EDGE('',*,*,#9096,.T.);
#12550=ORIENTED_EDGE('',*,*,#9011,.T.);
#12551=ORIENTED_EDGE('',*,*,#9097,.T.);
#12552=ORIENTED_EDGE('',*,*,#9098,.T.);
#12553=ORIENTED_EDGE('',*,*,#9094,.F.);
#12554=ORIENTED_EDGE('',*,*,#9099,.T.);
#12555=ORIENTED_EDGE('',*,*,#9029,.T.);
#12556=ORIENTED_EDGE('',*,*,#9100,.T.);
#12557=ORIENTED_EDGE('',*,*,#9097,.F.);
#12558=ORIENTED_EDGE('',*,*,#9101,.T.);
#12559=ORIENTED_EDGE('',*,*,#9059,.F.);
#12560=ORIENTED_EDGE('',*,*,#9102,.T.);
#12561=ORIENTED_EDGE('',*,*,#9030,.T.);
#12562=ORIENTED_EDGE('',*,*,#9102,.F.);
#12563=ORIENTED_EDGE('',*,*,#9058,.F.);
#12564=ORIENTED_EDGE('',*,*,#9103,.T.);
#12565=ORIENTED_EDGE('',*,*,#9031,.T.);
#12566=ORIENTED_EDGE('',*,*,#9103,.F.);
#12567=ORIENTED_EDGE('',*,*,#9057,.F.);
#12568=ORIENTED_EDGE('',*,*,#9022,.T.);
#12569=ORIENTED_EDGE('',*,*,#9036,.T.);
#12570=ORIENTED_EDGE('',*,*,#9043,.F.);
#12571=ORIENTED_EDGE('',*,*,#9049,.F.);
#12572=ORIENTED_EDGE('',*,*,#9104,.T.);
#12573=ORIENTED_EDGE('',*,*,#9037,.T.);
#12574=ORIENTED_EDGE('',*,*,#9104,.F.);
#12575=ORIENTED_EDGE('',*,*,#9048,.F.);
#12576=ORIENTED_EDGE('',*,*,#9105,.T.);
#12577=ORIENTED_EDGE('',*,*,#9090,.T.);
#12578=ORIENTED_EDGE('',*,*,#9106,.T.);
#12579=ORIENTED_EDGE('',*,*,#9038,.T.);
#12580=ORIENTED_EDGE('',*,*,#9105,.F.);
#12581=ORIENTED_EDGE('',*,*,#9047,.F.);
#12582=ORIENTED_EDGE('',*,*,#9107,.T.);
#12583=ORIENTED_EDGE('',*,*,#9063,.F.);
#12584=ORIENTED_EDGE('',*,*,#9108,.T.);
#12585=ORIENTED_EDGE('',*,*,#9109,.T.);
#12586=ORIENTED_EDGE('',*,*,#9110,.T.);
#12587=ORIENTED_EDGE('',*,*,#9111,.T.);
#12588=ORIENTED_EDGE('',*,*,#9112,.T.);
#12589=ORIENTED_EDGE('',*,*,#9071,.F.);
#12590=ORIENTED_EDGE('',*,*,#8992,.T.);
#12591=ORIENTED_EDGE('',*,*,#9113,.T.);
#12592=ORIENTED_EDGE('',*,*,#9114,.T.);
#12593=ORIENTED_EDGE('',*,*,#9065,.F.);
#12594=ORIENTED_EDGE('',*,*,#9112,.F.);
#12595=ORIENTED_EDGE('',*,*,#9109,.F.);
#12596=ORIENTED_EDGE('',*,*,#9115,.T.);
#12597=ORIENTED_EDGE('',*,*,#9116,.T.);
#12598=ORIENTED_EDGE('',*,*,#9117,.F.);
#12599=ORIENTED_EDGE('',*,*,#9118,.T.);
#12600=ORIENTED_EDGE('',*,*,#9119,.T.);
#12601=ORIENTED_EDGE('',*,*,#9113,.F.);
#12602=ORIENTED_EDGE('',*,*,#9111,.F.);
#12603=ORIENTED_EDGE('',*,*,#9117,.T.);
#12604=ORIENTED_EDGE('',*,*,#9120,.T.);
#12605=ORIENTED_EDGE('',*,*,#9118,.F.);
#12606=ORIENTED_EDGE('',*,*,#9110,.F.);
#12607=ORIENTED_EDGE('',*,*,#9121,.T.);
#12608=ORIENTED_EDGE('',*,*,#9122,.T.);
#12609=ORIENTED_EDGE('',*,*,#9061,.F.);
#12610=ORIENTED_EDGE('',*,*,#9070,.T.);
#12611=ORIENTED_EDGE('',*,*,#9123,.T.);
#12612=ORIENTED_EDGE('',*,*,#8984,.T.);
#12613=ORIENTED_EDGE('',*,*,#9124,.T.);
#12614=ORIENTED_EDGE('',*,*,#9125,.T.);
#12615=ORIENTED_EDGE('',*,*,#9121,.F.);
#12616=ORIENTED_EDGE('',*,*,#9126,.T.);
#12617=ORIENTED_EDGE('',*,*,#9069,.T.);
#12618=ORIENTED_EDGE('',*,*,#9127,.T.);
#12619=ORIENTED_EDGE('',*,*,#9126,.F.);
#12620=ORIENTED_EDGE('',*,*,#9123,.F.);
#12621=ORIENTED_EDGE('',*,*,#9056,.F.);
#12622=ORIENTED_EDGE('',*,*,#9128,.T.);
#12623=ORIENTED_EDGE('',*,*,#9074,.F.);
#12624=ORIENTED_EDGE('',*,*,#9129,.F.);
#12625=ORIENTED_EDGE('',*,*,#9129,.T.);
#12626=ORIENTED_EDGE('',*,*,#9073,.F.);
#12627=ORIENTED_EDGE('',*,*,#9130,.F.);
#12628=ORIENTED_EDGE('',*,*,#9020,.F.);
#12629=ORIENTED_EDGE('',*,*,#9075,.F.);
#12630=ORIENTED_EDGE('',*,*,#9131,.T.);
#12631=ORIENTED_EDGE('',*,*,#9124,.F.);
#12632=ORIENTED_EDGE('',*,*,#9132,.F.);
#12633=ORIENTED_EDGE('',*,*,#9130,.T.);
#12634=ORIENTED_EDGE('',*,*,#9072,.F.);
#12635=ORIENTED_EDGE('',*,*,#9133,.F.);
#12636=ORIENTED_EDGE('',*,*,#9032,.F.);
#12637=ORIENTED_EDGE('',*,*,#9085,.F.);
#12638=ORIENTED_EDGE('',*,*,#9134,.T.);
#12639=ORIENTED_EDGE('',*,*,#9050,.F.);
#12640=ORIENTED_EDGE('',*,*,#9135,.F.);
#12641=ORIENTED_EDGE('',*,*,#9132,.T.);
#12642=ORIENTED_EDGE('',*,*,#9127,.F.);
#12643=ORIENTED_EDGE('',*,*,#9136,.F.);
#12644=ORIENTED_EDGE('',*,*,#9076,.F.);
#12645=ORIENTED_EDGE('',*,*,#9137,.F.);
#12646=ORIENTED_EDGE('',*,*,#9133,.T.);
#12647=ORIENTED_EDGE('',*,*,#9138,.F.);
#12648=ORIENTED_EDGE('',*,*,#9135,.T.);
#12649=ORIENTED_EDGE('',*,*,#9041,.F.);
#12650=ORIENTED_EDGE('',*,*,#9139,.F.);
#12651=ORIENTED_EDGE('',*,*,#9086,.F.);
#12652=ORIENTED_EDGE('',*,*,#9116,.F.);
#12653=ORIENTED_EDGE('',*,*,#9140,.T.);
#12654=ORIENTED_EDGE('',*,*,#9084,.F.);
#12655=ORIENTED_EDGE('',*,*,#9141,.F.);
#12656=ORIENTED_EDGE('',*,*,#9136,.T.);
#12657=ORIENTED_EDGE('',*,*,#9068,.F.);
#12658=ORIENTED_EDGE('',*,*,#9142,.F.);
#12659=ORIENTED_EDGE('',*,*,#9077,.F.);
#12660=ORIENTED_EDGE('',*,*,#9138,.T.);
#12661=ORIENTED_EDGE('',*,*,#9078,.F.);
#12662=ORIENTED_EDGE('',*,*,#9143,.F.);
#12663=ORIENTED_EDGE('',*,*,#9023,.F.);
#12664=ORIENTED_EDGE('',*,*,#9137,.T.);
#12665=ORIENTED_EDGE('',*,*,#9026,.F.);
#12666=ORIENTED_EDGE('',*,*,#9144,.F.);
#12667=ORIENTED_EDGE('',*,*,#9033,.F.);
#12668=ORIENTED_EDGE('',*,*,#9139,.T.);
#12669=ORIENTED_EDGE('',*,*,#9034,.F.);
#12670=ORIENTED_EDGE('',*,*,#9145,.F.);
#12671=ORIENTED_EDGE('',*,*,#9087,.F.);
#12672=ORIENTED_EDGE('',*,*,#9141,.T.);
#12673=ORIENTED_EDGE('',*,*,#9083,.F.);
#12674=ORIENTED_EDGE('',*,*,#9146,.F.);
#12675=ORIENTED_EDGE('',*,*,#9120,.F.);
#12676=ORIENTED_EDGE('',*,*,#9143,.T.);
#12677=ORIENTED_EDGE('',*,*,#9142,.T.);
#12678=ORIENTED_EDGE('',*,*,#9147,.F.);
#12679=ORIENTED_EDGE('',*,*,#9145,.T.);
#12680=ORIENTED_EDGE('',*,*,#9144,.T.);
#12681=ORIENTED_EDGE('',*,*,#9148,.F.);
#12682=ORIENTED_EDGE('',*,*,#9146,.T.);
#12683=ORIENTED_EDGE('',*,*,#9082,.F.);
#12684=ORIENTED_EDGE('',*,*,#9149,.F.);
#12685=ORIENTED_EDGE('',*,*,#9119,.F.);
#12686=ORIENTED_EDGE('',*,*,#9147,.T.);
#12687=ORIENTED_EDGE('',*,*,#9067,.F.);
#12688=ORIENTED_EDGE('',*,*,#9150,.F.);
#12689=ORIENTED_EDGE('',*,*,#9024,.F.);
#12690=ORIENTED_EDGE('',*,*,#9148,.T.);
#12691=ORIENTED_EDGE('',*,*,#9025,.F.);
#12692=ORIENTED_EDGE('',*,*,#9151,.F.);
#12693=ORIENTED_EDGE('',*,*,#9079,.F.);
#12694=ORIENTED_EDGE('',*,*,#9149,.T.);
#12695=ORIENTED_EDGE('',*,*,#9081,.F.);
#12696=ORIENTED_EDGE('',*,*,#9152,.F.);
#12697=ORIENTED_EDGE('',*,*,#9114,.F.);
#12698=ORIENTED_EDGE('',*,*,#9151,.T.);
#12699=ORIENTED_EDGE('',*,*,#9150,.T.);
#12700=ORIENTED_EDGE('',*,*,#9153,.F.);
#12701=ORIENTED_EDGE('',*,*,#9152,.T.);
#12702=ORIENTED_EDGE('',*,*,#9080,.F.);
#12703=ORIENTED_EDGE('',*,*,#9153,.T.);
#12704=ORIENTED_EDGE('',*,*,#9066,.F.);
#12705=ORIENTED_EDGE('',*,*,#9131,.F.);
#12706=ORIENTED_EDGE('',*,*,#9128,.F.);
#12707=ORIENTED_EDGE('',*,*,#9154,.F.);
#12708=ORIENTED_EDGE('',*,*,#9154,.T.);
#12709=ORIENTED_EDGE('',*,*,#9055,.F.);
#12710=ORIENTED_EDGE('',*,*,#9155,.F.);
#12711=ORIENTED_EDGE('',*,*,#9125,.F.);
#12712=ORIENTED_EDGE('',*,*,#9155,.T.);
#12713=ORIENTED_EDGE('',*,*,#9054,.F.);
#12714=ORIENTED_EDGE('',*,*,#9156,.F.);
#12715=ORIENTED_EDGE('',*,*,#9122,.F.);
#12716=ORIENTED_EDGE('',*,*,#9156,.T.);
#12717=ORIENTED_EDGE('',*,*,#9053,.F.);
#12718=ORIENTED_EDGE('',*,*,#9157,.F.);
#12719=ORIENTED_EDGE('',*,*,#9062,.F.);
#12720=ORIENTED_EDGE('',*,*,#9157,.T.);
#12721=ORIENTED_EDGE('',*,*,#9052,.F.);
#12722=ORIENTED_EDGE('',*,*,#9158,.F.);
#12723=ORIENTED_EDGE('',*,*,#9108,.F.);
#12724=ORIENTED_EDGE('',*,*,#9158,.T.);
#12725=ORIENTED_EDGE('',*,*,#9051,.F.);
#12726=ORIENTED_EDGE('',*,*,#9159,.F.);
#12727=ORIENTED_EDGE('',*,*,#9115,.F.);
#12728=ORIENTED_EDGE('',*,*,#9159,.T.);
#12729=ORIENTED_EDGE('',*,*,#9134,.F.);
#12730=ORIENTED_EDGE('',*,*,#9140,.F.);
#12731=ORIENTED_EDGE('',*,*,#9100,.F.);
#12732=ORIENTED_EDGE('',*,*,#9028,.F.);
#12733=ORIENTED_EDGE('',*,*,#9095,.F.);
#12734=ORIENTED_EDGE('',*,*,#9098,.F.);
#12735=ORIENTED_EDGE('',*,*,#9092,.F.);
#12736=ORIENTED_EDGE('',*,*,#9039,.F.);
#12737=ORIENTED_EDGE('',*,*,#9106,.F.);
#12738=ORIENTED_EDGE('',*,*,#9089,.F.);
#12739=ORIENTED_EDGE('',*,*,#9101,.F.);
#12740=ORIENTED_EDGE('',*,*,#9099,.F.);
#12741=ORIENTED_EDGE('',*,*,#9096,.F.);
#12742=ORIENTED_EDGE('',*,*,#9060,.F.);
#12743=ORIENTED_EDGE('',*,*,#9093,.F.);
#12744=ORIENTED_EDGE('',*,*,#9091,.F.);
#12745=ORIENTED_EDGE('',*,*,#9107,.F.);
#12746=ORIENTED_EDGE('',*,*,#9046,.F.);
#12747=ORIENTED_EDGE('',*,*,#9160,.F.);
#12748=ORIENTED_EDGE('',*,*,#9161,.T.);
#12749=ORIENTED_EDGE('',*,*,#9162,.F.);
#12750=ORIENTED_EDGE('',*,*,#9163,.F.);
#12751=ORIENTED_EDGE('',*,*,#9161,.F.);
#12752=ORIENTED_EDGE('',*,*,#9164,.F.);
#12753=ORIENTED_EDGE('',*,*,#9165,.F.);
#12754=ORIENTED_EDGE('',*,*,#9166,.T.);
#12755=ORIENTED_EDGE('',*,*,#9167,.F.);
#12756=ORIENTED_EDGE('',*,*,#9166,.F.);
#12757=ORIENTED_EDGE('',*,*,#9164,.T.);
#12758=ORIENTED_EDGE('',*,*,#9165,.T.);
#12759=ORIENTED_EDGE('',*,*,#9168,.T.);
#12760=ORIENTED_EDGE('',*,*,#9162,.T.);
#12761=ORIENTED_EDGE('',*,*,#9163,.T.);
#12762=ORIENTED_EDGE('',*,*,#9168,.F.);
#12763=ORIENTED_EDGE('',*,*,#9160,.T.);
#12764=ORIENTED_EDGE('',*,*,#9167,.T.);
#12765=ORIENTED_EDGE('',*,*,#9169,.T.);
#12766=ORIENTED_EDGE('',*,*,#9170,.T.);
#12767=ORIENTED_EDGE('',*,*,#9171,.F.);
#12768=ORIENTED_EDGE('',*,*,#9170,.F.);
#12769=ORIENTED_EDGE('',*,*,#9172,.T.);
#12770=ORIENTED_EDGE('',*,*,#9173,.T.);
#12771=ORIENTED_EDGE('',*,*,#9174,.T.);
#12772=ORIENTED_EDGE('',*,*,#9175,.F.);
#12773=ORIENTED_EDGE('',*,*,#9174,.F.);
#12774=ORIENTED_EDGE('',*,*,#9176,.T.);
#12775=ORIENTED_EDGE('',*,*,#9177,.F.);
#12776=ORIENTED_EDGE('',*,*,#9178,.T.);
#12777=ORIENTED_EDGE('',*,*,#9179,.T.);
#12778=ORIENTED_EDGE('',*,*,#9178,.F.);
#12779=ORIENTED_EDGE('',*,*,#9180,.F.);
#12780=ORIENTED_EDGE('',*,*,#9181,.T.);
#12781=ORIENTED_EDGE('',*,*,#9182,.F.);
#12782=ORIENTED_EDGE('',*,*,#9181,.F.);
#12783=ORIENTED_EDGE('',*,*,#9183,.T.);
#12784=ORIENTED_EDGE('',*,*,#9184,.T.);
#12785=ORIENTED_EDGE('',*,*,#9185,.F.);
#12786=ORIENTED_EDGE('',*,*,#9184,.F.);
#12787=ORIENTED_EDGE('',*,*,#9186,.F.);
#12788=ORIENTED_EDGE('',*,*,#9187,.T.);
#12789=ORIENTED_EDGE('',*,*,#9188,.F.);
#12790=ORIENTED_EDGE('',*,*,#9187,.F.);
#12791=ORIENTED_EDGE('',*,*,#9172,.F.);
#12792=ORIENTED_EDGE('',*,*,#9189,.F.);
#12793=ORIENTED_EDGE('',*,*,#9190,.F.);
#12794=ORIENTED_EDGE('',*,*,#9191,.T.);
#12795=ORIENTED_EDGE('',*,*,#9192,.T.);
#12796=ORIENTED_EDGE('',*,*,#9193,.T.);
#12797=ORIENTED_EDGE('',*,*,#9194,.F.);
#12798=ORIENTED_EDGE('',*,*,#9195,.F.);
#12799=ORIENTED_EDGE('',*,*,#9194,.T.);
#12800=ORIENTED_EDGE('',*,*,#9196,.T.);
#12801=ORIENTED_EDGE('',*,*,#9197,.F.);
#12802=ORIENTED_EDGE('',*,*,#9198,.F.);
#12803=ORIENTED_EDGE('',*,*,#9190,.T.);
#12804=ORIENTED_EDGE('',*,*,#9199,.T.);
#12805=ORIENTED_EDGE('',*,*,#9195,.T.);
#12806=ORIENTED_EDGE('',*,*,#9198,.T.);
#12807=ORIENTED_EDGE('',*,*,#9200,.T.);
#12808=ORIENTED_EDGE('',*,*,#9183,.F.);
#12809=ORIENTED_EDGE('',*,*,#9201,.F.);
#12810=ORIENTED_EDGE('',*,*,#9202,.F.);
#12811=ORIENTED_EDGE('',*,*,#9203,.F.);
#12812=ORIENTED_EDGE('',*,*,#9204,.F.);
#12813=ORIENTED_EDGE('',*,*,#9205,.F.);
#12814=ORIENTED_EDGE('',*,*,#9182,.T.);
#12815=ORIENTED_EDGE('',*,*,#9173,.F.);
#12816=ORIENTED_EDGE('',*,*,#9206,.T.);
#12817=ORIENTED_EDGE('',*,*,#9201,.T.);
#12818=ORIENTED_EDGE('',*,*,#9207,.F.);
#12819=ORIENTED_EDGE('',*,*,#9176,.F.);
#12820=ORIENTED_EDGE('',*,*,#9208,.F.);
#12821=ORIENTED_EDGE('',*,*,#9209,.F.);
#12822=ORIENTED_EDGE('',*,*,#9192,.F.);
#12823=ORIENTED_EDGE('',*,*,#9199,.F.);
#12824=ORIENTED_EDGE('',*,*,#9189,.T.);
#12825=ORIENTED_EDGE('',*,*,#9207,.T.);
#12826=ORIENTED_EDGE('',*,*,#9205,.T.);
#12827=ORIENTED_EDGE('',*,*,#9210,.F.);
#12828=ORIENTED_EDGE('',*,*,#9211,.F.);
#12829=ORIENTED_EDGE('',*,*,#9186,.T.);
#12830=ORIENTED_EDGE('',*,*,#9212,.F.);
#12831=ORIENTED_EDGE('',*,*,#9213,.T.);
#12832=ORIENTED_EDGE('',*,*,#9210,.T.);
#12833=ORIENTED_EDGE('',*,*,#9204,.T.);
#12834=ORIENTED_EDGE('',*,*,#9214,.F.);
#12835=ORIENTED_EDGE('',*,*,#9215,.T.);
#12836=ORIENTED_EDGE('',*,*,#9212,.T.);
#12837=ORIENTED_EDGE('',*,*,#9203,.T.);
#12838=ORIENTED_EDGE('',*,*,#9197,.T.);
#12839=ORIENTED_EDGE('',*,*,#9216,.T.);
#12840=ORIENTED_EDGE('',*,*,#9217,.T.);
#12841=ORIENTED_EDGE('',*,*,#9218,.T.);
#12842=ORIENTED_EDGE('',*,*,#9214,.T.);
#12843=ORIENTED_EDGE('',*,*,#9202,.T.);
#12844=ORIENTED_EDGE('',*,*,#9206,.F.);
#12845=ORIENTED_EDGE('',*,*,#9191,.F.);
#12846=ORIENTED_EDGE('',*,*,#9200,.F.);
#12847=ORIENTED_EDGE('',*,*,#9179,.F.);
#12848=ORIENTED_EDGE('',*,*,#9209,.T.);
#12849=ORIENTED_EDGE('',*,*,#9219,.F.);
#12850=ORIENTED_EDGE('',*,*,#9216,.F.);
#12851=ORIENTED_EDGE('',*,*,#9196,.F.);
#12852=ORIENTED_EDGE('',*,*,#9193,.F.);
#12853=ORIENTED_EDGE('',*,*,#9185,.T.);
#12854=ORIENTED_EDGE('',*,*,#9215,.F.);
#12855=ORIENTED_EDGE('',*,*,#9218,.F.);
#12856=ORIENTED_EDGE('',*,*,#9220,.T.);
#12857=ORIENTED_EDGE('',*,*,#9211,.T.);
#12858=ORIENTED_EDGE('',*,*,#9213,.F.);
#12859=ORIENTED_EDGE('',*,*,#9180,.T.);
#12860=ORIENTED_EDGE('',*,*,#9208,.T.);
#12861=ORIENTED_EDGE('',*,*,#9220,.F.);
#12862=ORIENTED_EDGE('',*,*,#9217,.F.);
#12863=ORIENTED_EDGE('',*,*,#9219,.T.);
#12864=ORIENTED_EDGE('',*,*,#9177,.T.);
#12865=ORIENTED_EDGE('',*,*,#9188,.T.);
#12866=ORIENTED_EDGE('',*,*,#9175,.T.);
#12867=ORIENTED_EDGE('',*,*,#9169,.F.);
#12868=ORIENTED_EDGE('',*,*,#9171,.T.);
#12869=ORIENTED_EDGE('',*,*,#9221,.F.);
#12870=ORIENTED_EDGE('',*,*,#9222,.T.);
#12871=ORIENTED_EDGE('',*,*,#9223,.T.);
#12872=ORIENTED_EDGE('',*,*,#9222,.F.);
#12873=ORIENTED_EDGE('',*,*,#9224,.T.);
#12874=ORIENTED_EDGE('',*,*,#9224,.F.);
#12875=ORIENTED_EDGE('',*,*,#9221,.T.);
#12876=ORIENTED_EDGE('',*,*,#9223,.F.);
#12877=ORIENTED_EDGE('',*,*,#9225,.F.);
#12878=ORIENTED_EDGE('',*,*,#9226,.T.);
#12879=ORIENTED_EDGE('',*,*,#9227,.F.);
#12880=ORIENTED_EDGE('',*,*,#9226,.F.);
#12881=ORIENTED_EDGE('',*,*,#9228,.F.);
#12882=ORIENTED_EDGE('',*,*,#9229,.F.);
#12883=ORIENTED_EDGE('',*,*,#9230,.T.);
#12884=ORIENTED_EDGE('',*,*,#9231,.T.);
#12885=ORIENTED_EDGE('',*,*,#9230,.F.);
#12886=ORIENTED_EDGE('',*,*,#9232,.F.);
#12887=ORIENTED_EDGE('',*,*,#9233,.F.);
#12888=ORIENTED_EDGE('',*,*,#9234,.T.);
#12889=ORIENTED_EDGE('',*,*,#9235,.T.);
#12890=ORIENTED_EDGE('',*,*,#9236,.T.);
#12891=ORIENTED_EDGE('',*,*,#9234,.F.);
#12892=ORIENTED_EDGE('',*,*,#9228,.T.);
#12893=ORIENTED_EDGE('',*,*,#9229,.T.);
#12894=ORIENTED_EDGE('',*,*,#9237,.T.);
#12895=ORIENTED_EDGE('',*,*,#9235,.F.);
#12896=ORIENTED_EDGE('',*,*,#9236,.F.);
#12897=ORIENTED_EDGE('',*,*,#9237,.F.);
#12898=ORIENTED_EDGE('',*,*,#9238,.F.);
#12899=ORIENTED_EDGE('',*,*,#9239,.F.);
#12900=ORIENTED_EDGE('',*,*,#9240,.T.);
#12901=ORIENTED_EDGE('',*,*,#9232,.T.);
#12902=ORIENTED_EDGE('',*,*,#9233,.T.);
#12903=ORIENTED_EDGE('',*,*,#9240,.F.);
#12904=ORIENTED_EDGE('',*,*,#9241,.F.);
#12905=ORIENTED_EDGE('',*,*,#9242,.F.);
#12906=ORIENTED_EDGE('',*,*,#9243,.T.);
#12907=ORIENTED_EDGE('',*,*,#9244,.T.);
#12908=ORIENTED_EDGE('',*,*,#9245,.T.);
#12909=ORIENTED_EDGE('',*,*,#9243,.F.);
#12910=ORIENTED_EDGE('',*,*,#9238,.T.);
#12911=ORIENTED_EDGE('',*,*,#9239,.T.);
#12912=ORIENTED_EDGE('',*,*,#9246,.T.);
#12913=ORIENTED_EDGE('',*,*,#9244,.F.);
#12914=ORIENTED_EDGE('',*,*,#9245,.F.);
#12915=ORIENTED_EDGE('',*,*,#9246,.F.);
#12916=ORIENTED_EDGE('',*,*,#9247,.F.);
#12917=ORIENTED_EDGE('',*,*,#9248,.F.);
#12918=ORIENTED_EDGE('',*,*,#9249,.T.);
#12919=ORIENTED_EDGE('',*,*,#9241,.T.);
#12920=ORIENTED_EDGE('',*,*,#9242,.T.);
#12921=ORIENTED_EDGE('',*,*,#9249,.F.);
#12922=ORIENTED_EDGE('',*,*,#9250,.F.);
#12923=ORIENTED_EDGE('',*,*,#9251,.F.);
#12924=ORIENTED_EDGE('',*,*,#9252,.T.);
#12925=ORIENTED_EDGE('',*,*,#9253,.T.);
#12926=ORIENTED_EDGE('',*,*,#9254,.T.);
#12927=ORIENTED_EDGE('',*,*,#9252,.F.);
#12928=ORIENTED_EDGE('',*,*,#9247,.T.);
#12929=ORIENTED_EDGE('',*,*,#9248,.T.);
#12930=ORIENTED_EDGE('',*,*,#9255,.T.);
#12931=ORIENTED_EDGE('',*,*,#9253,.F.);
#12932=ORIENTED_EDGE('',*,*,#9254,.F.);
#12933=ORIENTED_EDGE('',*,*,#9255,.F.);
#12934=ORIENTED_EDGE('',*,*,#9256,.F.);
#12935=ORIENTED_EDGE('',*,*,#9257,.F.);
#12936=ORIENTED_EDGE('',*,*,#9258,.T.);
#12937=ORIENTED_EDGE('',*,*,#9250,.T.);
#12938=ORIENTED_EDGE('',*,*,#9251,.T.);
#12939=ORIENTED_EDGE('',*,*,#9258,.F.);
#12940=ORIENTED_EDGE('',*,*,#9259,.F.);
#12941=ORIENTED_EDGE('',*,*,#9260,.F.);
#12942=ORIENTED_EDGE('',*,*,#9261,.T.);
#12943=ORIENTED_EDGE('',*,*,#9262,.T.);
#12944=ORIENTED_EDGE('',*,*,#9263,.T.);
#12945=ORIENTED_EDGE('',*,*,#9261,.F.);
#12946=ORIENTED_EDGE('',*,*,#9256,.T.);
#12947=ORIENTED_EDGE('',*,*,#9257,.T.);
#12948=ORIENTED_EDGE('',*,*,#9264,.T.);
#12949=ORIENTED_EDGE('',*,*,#9262,.F.);
#12950=ORIENTED_EDGE('',*,*,#9263,.F.);
#12951=ORIENTED_EDGE('',*,*,#9264,.F.);
#12952=ORIENTED_EDGE('',*,*,#9265,.F.);
#12953=ORIENTED_EDGE('',*,*,#9266,.F.);
#12954=ORIENTED_EDGE('',*,*,#9267,.T.);
#12955=ORIENTED_EDGE('',*,*,#9259,.T.);
#12956=ORIENTED_EDGE('',*,*,#9260,.T.);
#12957=ORIENTED_EDGE('',*,*,#9267,.F.);
#12958=ORIENTED_EDGE('',*,*,#9268,.F.);
#12959=ORIENTED_EDGE('',*,*,#9269,.F.);
#12960=ORIENTED_EDGE('',*,*,#9270,.T.);
#12961=ORIENTED_EDGE('',*,*,#9271,.T.);
#12962=ORIENTED_EDGE('',*,*,#9272,.T.);
#12963=ORIENTED_EDGE('',*,*,#9270,.F.);
#12964=ORIENTED_EDGE('',*,*,#9265,.T.);
#12965=ORIENTED_EDGE('',*,*,#9266,.T.);
#12966=ORIENTED_EDGE('',*,*,#9273,.T.);
#12967=ORIENTED_EDGE('',*,*,#9271,.F.);
#12968=ORIENTED_EDGE('',*,*,#9272,.F.);
#12969=ORIENTED_EDGE('',*,*,#9273,.F.);
#12970=ORIENTED_EDGE('',*,*,#9274,.F.);
#12971=ORIENTED_EDGE('',*,*,#9275,.F.);
#12972=ORIENTED_EDGE('',*,*,#9276,.T.);
#12973=ORIENTED_EDGE('',*,*,#9268,.T.);
#12974=ORIENTED_EDGE('',*,*,#9269,.T.);
#12975=ORIENTED_EDGE('',*,*,#9276,.F.);
#12976=ORIENTED_EDGE('',*,*,#9277,.F.);
#12977=ORIENTED_EDGE('',*,*,#9278,.F.);
#12978=ORIENTED_EDGE('',*,*,#9279,.T.);
#12979=ORIENTED_EDGE('',*,*,#9280,.T.);
#12980=ORIENTED_EDGE('',*,*,#9281,.T.);
#12981=ORIENTED_EDGE('',*,*,#9279,.F.);
#12982=ORIENTED_EDGE('',*,*,#9274,.T.);
#12983=ORIENTED_EDGE('',*,*,#9275,.T.);
#12984=ORIENTED_EDGE('',*,*,#9282,.T.);
#12985=ORIENTED_EDGE('',*,*,#9280,.F.);
#12986=ORIENTED_EDGE('',*,*,#9281,.F.);
#12987=ORIENTED_EDGE('',*,*,#9282,.F.);
#12988=ORIENTED_EDGE('',*,*,#9283,.F.);
#12989=ORIENTED_EDGE('',*,*,#9284,.F.);
#12990=ORIENTED_EDGE('',*,*,#9285,.T.);
#12991=ORIENTED_EDGE('',*,*,#9277,.T.);
#12992=ORIENTED_EDGE('',*,*,#9278,.T.);
#12993=ORIENTED_EDGE('',*,*,#9285,.F.);
#12994=ORIENTED_EDGE('',*,*,#9286,.F.);
#12995=ORIENTED_EDGE('',*,*,#9287,.F.);
#12996=ORIENTED_EDGE('',*,*,#9288,.T.);
#12997=ORIENTED_EDGE('',*,*,#9289,.T.);
#12998=ORIENTED_EDGE('',*,*,#9290,.T.);
#12999=ORIENTED_EDGE('',*,*,#9288,.F.);
#13000=ORIENTED_EDGE('',*,*,#9283,.T.);
#13001=ORIENTED_EDGE('',*,*,#9284,.T.);
#13002=ORIENTED_EDGE('',*,*,#9291,.T.);
#13003=ORIENTED_EDGE('',*,*,#9289,.F.);
#13004=ORIENTED_EDGE('',*,*,#9290,.F.);
#13005=ORIENTED_EDGE('',*,*,#9291,.F.);
#13006=ORIENTED_EDGE('',*,*,#9292,.F.);
#13007=ORIENTED_EDGE('',*,*,#9293,.F.);
#13008=ORIENTED_EDGE('',*,*,#9294,.T.);
#13009=ORIENTED_EDGE('',*,*,#9286,.T.);
#13010=ORIENTED_EDGE('',*,*,#9287,.T.);
#13011=ORIENTED_EDGE('',*,*,#9294,.F.);
#13012=ORIENTED_EDGE('',*,*,#9295,.F.);
#13013=ORIENTED_EDGE('',*,*,#9296,.F.);
#13014=ORIENTED_EDGE('',*,*,#9297,.T.);
#13015=ORIENTED_EDGE('',*,*,#9298,.T.);
#13016=ORIENTED_EDGE('',*,*,#9299,.T.);
#13017=ORIENTED_EDGE('',*,*,#9297,.F.);
#13018=ORIENTED_EDGE('',*,*,#9292,.T.);
#13019=ORIENTED_EDGE('',*,*,#9293,.T.);
#13020=ORIENTED_EDGE('',*,*,#9300,.T.);
#13021=ORIENTED_EDGE('',*,*,#9298,.F.);
#13022=ORIENTED_EDGE('',*,*,#9299,.F.);
#13023=ORIENTED_EDGE('',*,*,#9300,.F.);
#13024=ORIENTED_EDGE('',*,*,#9301,.F.);
#13025=ORIENTED_EDGE('',*,*,#9302,.F.);
#13026=ORIENTED_EDGE('',*,*,#9303,.T.);
#13027=ORIENTED_EDGE('',*,*,#9295,.T.);
#13028=ORIENTED_EDGE('',*,*,#9296,.T.);
#13029=ORIENTED_EDGE('',*,*,#9303,.F.);
#13030=ORIENTED_EDGE('',*,*,#9304,.F.);
#13031=ORIENTED_EDGE('',*,*,#9305,.F.);
#13032=ORIENTED_EDGE('',*,*,#9306,.T.);
#13033=ORIENTED_EDGE('',*,*,#9307,.T.);
#13034=ORIENTED_EDGE('',*,*,#9308,.T.);
#13035=ORIENTED_EDGE('',*,*,#9306,.F.);
#13036=ORIENTED_EDGE('',*,*,#9301,.T.);
#13037=ORIENTED_EDGE('',*,*,#9302,.T.);
#13038=ORIENTED_EDGE('',*,*,#9309,.T.);
#13039=ORIENTED_EDGE('',*,*,#9307,.F.);
#13040=ORIENTED_EDGE('',*,*,#9308,.F.);
#13041=ORIENTED_EDGE('',*,*,#9309,.F.);
#13042=ORIENTED_EDGE('',*,*,#9310,.F.);
#13043=ORIENTED_EDGE('',*,*,#9311,.F.);
#13044=ORIENTED_EDGE('',*,*,#9312,.T.);
#13045=ORIENTED_EDGE('',*,*,#9304,.T.);
#13046=ORIENTED_EDGE('',*,*,#9305,.T.);
#13047=ORIENTED_EDGE('',*,*,#9312,.F.);
#13048=ORIENTED_EDGE('',*,*,#9313,.F.);
#13049=ORIENTED_EDGE('',*,*,#9314,.F.);
#13050=ORIENTED_EDGE('',*,*,#9315,.T.);
#13051=ORIENTED_EDGE('',*,*,#9316,.T.);
#13052=ORIENTED_EDGE('',*,*,#9317,.T.);
#13053=ORIENTED_EDGE('',*,*,#9315,.F.);
#13054=ORIENTED_EDGE('',*,*,#9310,.T.);
#13055=ORIENTED_EDGE('',*,*,#9311,.T.);
#13056=ORIENTED_EDGE('',*,*,#9318,.T.);
#13057=ORIENTED_EDGE('',*,*,#9316,.F.);
#13058=ORIENTED_EDGE('',*,*,#9317,.F.);
#13059=ORIENTED_EDGE('',*,*,#9318,.F.);
#13060=ORIENTED_EDGE('',*,*,#9319,.F.);
#13061=ORIENTED_EDGE('',*,*,#9320,.F.);
#13062=ORIENTED_EDGE('',*,*,#9321,.T.);
#13063=ORIENTED_EDGE('',*,*,#9313,.T.);
#13064=ORIENTED_EDGE('',*,*,#9314,.T.);
#13065=ORIENTED_EDGE('',*,*,#9321,.F.);
#13066=ORIENTED_EDGE('',*,*,#9322,.F.);
#13067=ORIENTED_EDGE('',*,*,#9323,.F.);
#13068=ORIENTED_EDGE('',*,*,#9324,.T.);
#13069=ORIENTED_EDGE('',*,*,#9325,.T.);
#13070=ORIENTED_EDGE('',*,*,#9326,.T.);
#13071=ORIENTED_EDGE('',*,*,#9324,.F.);
#13072=ORIENTED_EDGE('',*,*,#9319,.T.);
#13073=ORIENTED_EDGE('',*,*,#9320,.T.);
#13074=ORIENTED_EDGE('',*,*,#9327,.T.);
#13075=ORIENTED_EDGE('',*,*,#9325,.F.);
#13076=ORIENTED_EDGE('',*,*,#9326,.F.);
#13077=ORIENTED_EDGE('',*,*,#9327,.F.);
#13078=ORIENTED_EDGE('',*,*,#9328,.F.);
#13079=ORIENTED_EDGE('',*,*,#9329,.F.);
#13080=ORIENTED_EDGE('',*,*,#9330,.T.);
#13081=ORIENTED_EDGE('',*,*,#9322,.T.);
#13082=ORIENTED_EDGE('',*,*,#9323,.T.);
#13083=ORIENTED_EDGE('',*,*,#9330,.F.);
#13084=ORIENTED_EDGE('',*,*,#9331,.F.);
#13085=ORIENTED_EDGE('',*,*,#9332,.F.);
#13086=ORIENTED_EDGE('',*,*,#9333,.T.);
#13087=ORIENTED_EDGE('',*,*,#9334,.T.);
#13088=ORIENTED_EDGE('',*,*,#9335,.T.);
#13089=ORIENTED_EDGE('',*,*,#9333,.F.);
#13090=ORIENTED_EDGE('',*,*,#9328,.T.);
#13091=ORIENTED_EDGE('',*,*,#9329,.T.);
#13092=ORIENTED_EDGE('',*,*,#9336,.T.);
#13093=ORIENTED_EDGE('',*,*,#9334,.F.);
#13094=ORIENTED_EDGE('',*,*,#9335,.F.);
#13095=ORIENTED_EDGE('',*,*,#9336,.F.);
#13096=ORIENTED_EDGE('',*,*,#9337,.F.);
#13097=ORIENTED_EDGE('',*,*,#9338,.F.);
#13098=ORIENTED_EDGE('',*,*,#9339,.T.);
#13099=ORIENTED_EDGE('',*,*,#9331,.T.);
#13100=ORIENTED_EDGE('',*,*,#9332,.T.);
#13101=ORIENTED_EDGE('',*,*,#9339,.F.);
#13102=ORIENTED_EDGE('',*,*,#9340,.F.);
#13103=ORIENTED_EDGE('',*,*,#9341,.F.);
#13104=ORIENTED_EDGE('',*,*,#9342,.T.);
#13105=ORIENTED_EDGE('',*,*,#9343,.T.);
#13106=ORIENTED_EDGE('',*,*,#9344,.T.);
#13107=ORIENTED_EDGE('',*,*,#9342,.F.);
#13108=ORIENTED_EDGE('',*,*,#9337,.T.);
#13109=ORIENTED_EDGE('',*,*,#9338,.T.);
#13110=ORIENTED_EDGE('',*,*,#9345,.T.);
#13111=ORIENTED_EDGE('',*,*,#9343,.F.);
#13112=ORIENTED_EDGE('',*,*,#9344,.F.);
#13113=ORIENTED_EDGE('',*,*,#9345,.F.);
#13114=ORIENTED_EDGE('',*,*,#9346,.F.);
#13115=ORIENTED_EDGE('',*,*,#9347,.F.);
#13116=ORIENTED_EDGE('',*,*,#9348,.T.);
#13117=ORIENTED_EDGE('',*,*,#9340,.T.);
#13118=ORIENTED_EDGE('',*,*,#9341,.T.);
#13119=ORIENTED_EDGE('',*,*,#9348,.F.);
#13120=ORIENTED_EDGE('',*,*,#9349,.F.);
#13121=ORIENTED_EDGE('',*,*,#9350,.F.);
#13122=ORIENTED_EDGE('',*,*,#9351,.T.);
#13123=ORIENTED_EDGE('',*,*,#9352,.T.);
#13124=ORIENTED_EDGE('',*,*,#9353,.T.);
#13125=ORIENTED_EDGE('',*,*,#9351,.F.);
#13126=ORIENTED_EDGE('',*,*,#9346,.T.);
#13127=ORIENTED_EDGE('',*,*,#9347,.T.);
#13128=ORIENTED_EDGE('',*,*,#9354,.T.);
#13129=ORIENTED_EDGE('',*,*,#9352,.F.);
#13130=ORIENTED_EDGE('',*,*,#9353,.F.);
#13131=ORIENTED_EDGE('',*,*,#9354,.F.);
#13132=ORIENTED_EDGE('',*,*,#9355,.F.);
#13133=ORIENTED_EDGE('',*,*,#9356,.F.);
#13134=ORIENTED_EDGE('',*,*,#9357,.T.);
#13135=ORIENTED_EDGE('',*,*,#9349,.T.);
#13136=ORIENTED_EDGE('',*,*,#9350,.T.);
#13137=ORIENTED_EDGE('',*,*,#9357,.F.);
#13138=ORIENTED_EDGE('',*,*,#9358,.F.);
#13139=ORIENTED_EDGE('',*,*,#9359,.F.);
#13140=ORIENTED_EDGE('',*,*,#9360,.T.);
#13141=ORIENTED_EDGE('',*,*,#9361,.T.);
#13142=ORIENTED_EDGE('',*,*,#9362,.T.);
#13143=ORIENTED_EDGE('',*,*,#9360,.F.);
#13144=ORIENTED_EDGE('',*,*,#9355,.T.);
#13145=ORIENTED_EDGE('',*,*,#9356,.T.);
#13146=ORIENTED_EDGE('',*,*,#9363,.T.);
#13147=ORIENTED_EDGE('',*,*,#9361,.F.);
#13148=ORIENTED_EDGE('',*,*,#9362,.F.);
#13149=ORIENTED_EDGE('',*,*,#9363,.F.);
#13150=ORIENTED_EDGE('',*,*,#9364,.F.);
#13151=ORIENTED_EDGE('',*,*,#9365,.T.);
#13152=ORIENTED_EDGE('',*,*,#9366,.F.);
#13153=ORIENTED_EDGE('',*,*,#9367,.F.);
#13154=ORIENTED_EDGE('',*,*,#9368,.T.);
#13155=ORIENTED_EDGE('',*,*,#9369,.F.);
#13156=ORIENTED_EDGE('',*,*,#9370,.F.);
#13157=ORIENTED_EDGE('',*,*,#9371,.T.);
#13158=ORIENTED_EDGE('',*,*,#9372,.F.);
#13159=ORIENTED_EDGE('',*,*,#9373,.F.);
#13160=ORIENTED_EDGE('',*,*,#9374,.T.);
#13161=ORIENTED_EDGE('',*,*,#9375,.F.);
#13162=ORIENTED_EDGE('',*,*,#9376,.F.);
#13163=ORIENTED_EDGE('',*,*,#9377,.T.);
#13164=ORIENTED_EDGE('',*,*,#9378,.F.);
#13165=ORIENTED_EDGE('',*,*,#9379,.F.);
#13166=ORIENTED_EDGE('',*,*,#9380,.T.);
#13167=ORIENTED_EDGE('',*,*,#9381,.F.);
#13168=ORIENTED_EDGE('',*,*,#9382,.F.);
#13169=ORIENTED_EDGE('',*,*,#9383,.T.);
#13170=ORIENTED_EDGE('',*,*,#9384,.F.);
#13171=ORIENTED_EDGE('',*,*,#9385,.F.);
#13172=ORIENTED_EDGE('',*,*,#9386,.T.);
#13173=ORIENTED_EDGE('',*,*,#9387,.F.);
#13174=ORIENTED_EDGE('',*,*,#9388,.F.);
#13175=ORIENTED_EDGE('',*,*,#9389,.T.);
#13176=ORIENTED_EDGE('',*,*,#9390,.F.);
#13177=ORIENTED_EDGE('',*,*,#9391,.F.);
#13178=ORIENTED_EDGE('',*,*,#9392,.T.);
#13179=ORIENTED_EDGE('',*,*,#9393,.F.);
#13180=ORIENTED_EDGE('',*,*,#9394,.F.);
#13181=ORIENTED_EDGE('',*,*,#9395,.T.);
#13182=ORIENTED_EDGE('',*,*,#9396,.F.);
#13183=ORIENTED_EDGE('',*,*,#9397,.F.);
#13184=ORIENTED_EDGE('',*,*,#9398,.T.);
#13185=ORIENTED_EDGE('',*,*,#9399,.F.);
#13186=ORIENTED_EDGE('',*,*,#9400,.F.);
#13187=ORIENTED_EDGE('',*,*,#9401,.T.);
#13188=ORIENTED_EDGE('',*,*,#9402,.F.);
#13189=ORIENTED_EDGE('',*,*,#9403,.F.);
#13190=ORIENTED_EDGE('',*,*,#9404,.T.);
#13191=ORIENTED_EDGE('',*,*,#9405,.F.);
#13192=ORIENTED_EDGE('',*,*,#9406,.F.);
#13193=ORIENTED_EDGE('',*,*,#9407,.T.);
#13194=ORIENTED_EDGE('',*,*,#9408,.F.);
#13195=ORIENTED_EDGE('',*,*,#9409,.F.);
#13196=ORIENTED_EDGE('',*,*,#9410,.T.);
#13197=ORIENTED_EDGE('',*,*,#9411,.F.);
#13198=ORIENTED_EDGE('',*,*,#9412,.F.);
#13199=ORIENTED_EDGE('',*,*,#9413,.T.);
#13200=ORIENTED_EDGE('',*,*,#9414,.F.);
#13201=ORIENTED_EDGE('',*,*,#9415,.F.);
#13202=ORIENTED_EDGE('',*,*,#9416,.T.);
#13203=ORIENTED_EDGE('',*,*,#9417,.F.);
#13204=ORIENTED_EDGE('',*,*,#9418,.F.);
#13205=ORIENTED_EDGE('',*,*,#9419,.T.);
#13206=ORIENTED_EDGE('',*,*,#9420,.F.);
#13207=ORIENTED_EDGE('',*,*,#9421,.F.);
#13208=ORIENTED_EDGE('',*,*,#9422,.T.);
#13209=ORIENTED_EDGE('',*,*,#9423,.F.);
#13210=ORIENTED_EDGE('',*,*,#9424,.F.);
#13211=ORIENTED_EDGE('',*,*,#9425,.T.);
#13212=ORIENTED_EDGE('',*,*,#9426,.F.);
#13213=ORIENTED_EDGE('',*,*,#9427,.F.);
#13214=ORIENTED_EDGE('',*,*,#9428,.T.);
#13215=ORIENTED_EDGE('',*,*,#9429,.F.);
#13216=ORIENTED_EDGE('',*,*,#9430,.F.);
#13217=ORIENTED_EDGE('',*,*,#9431,.T.);
#13218=ORIENTED_EDGE('',*,*,#9432,.F.);
#13219=ORIENTED_EDGE('',*,*,#9433,.F.);
#13220=ORIENTED_EDGE('',*,*,#9434,.T.);
#13221=ORIENTED_EDGE('',*,*,#9435,.F.);
#13222=ORIENTED_EDGE('',*,*,#9436,.F.);
#13223=ORIENTED_EDGE('',*,*,#9437,.T.);
#13224=ORIENTED_EDGE('',*,*,#9438,.F.);
#13225=ORIENTED_EDGE('',*,*,#9439,.F.);
#13226=ORIENTED_EDGE('',*,*,#9440,.T.);
#13227=ORIENTED_EDGE('',*,*,#9441,.F.);
#13228=ORIENTED_EDGE('',*,*,#9442,.F.);
#13229=ORIENTED_EDGE('',*,*,#9443,.T.);
#13230=ORIENTED_EDGE('',*,*,#9444,.F.);
#13231=ORIENTED_EDGE('',*,*,#9445,.F.);
#13232=ORIENTED_EDGE('',*,*,#9446,.T.);
#13233=ORIENTED_EDGE('',*,*,#9447,.F.);
#13234=ORIENTED_EDGE('',*,*,#9448,.F.);
#13235=ORIENTED_EDGE('',*,*,#9449,.T.);
#13236=ORIENTED_EDGE('',*,*,#9450,.F.);
#13237=ORIENTED_EDGE('',*,*,#9451,.F.);
#13238=ORIENTED_EDGE('',*,*,#9452,.T.);
#13239=ORIENTED_EDGE('',*,*,#9453,.F.);
#13240=ORIENTED_EDGE('',*,*,#9454,.F.);
#13241=ORIENTED_EDGE('',*,*,#9455,.T.);
#13242=ORIENTED_EDGE('',*,*,#9456,.F.);
#13243=ORIENTED_EDGE('',*,*,#9457,.F.);
#13244=ORIENTED_EDGE('',*,*,#9458,.T.);
#13245=ORIENTED_EDGE('',*,*,#9459,.F.);
#13246=ORIENTED_EDGE('',*,*,#9460,.F.);
#13247=ORIENTED_EDGE('',*,*,#9461,.T.);
#13248=ORIENTED_EDGE('',*,*,#9462,.F.);
#13249=ORIENTED_EDGE('',*,*,#9463,.F.);
#13250=ORIENTED_EDGE('',*,*,#9464,.T.);
#13251=ORIENTED_EDGE('',*,*,#9465,.F.);
#13252=ORIENTED_EDGE('',*,*,#9466,.F.);
#13253=ORIENTED_EDGE('',*,*,#9467,.T.);
#13254=ORIENTED_EDGE('',*,*,#9468,.F.);
#13255=ORIENTED_EDGE('',*,*,#9469,.F.);
#13256=ORIENTED_EDGE('',*,*,#9470,.T.);
#13257=ORIENTED_EDGE('',*,*,#9471,.F.);
#13258=ORIENTED_EDGE('',*,*,#9472,.F.);
#13259=ORIENTED_EDGE('',*,*,#9473,.T.);
#13260=ORIENTED_EDGE('',*,*,#9474,.F.);
#13261=ORIENTED_EDGE('',*,*,#9475,.F.);
#13262=ORIENTED_EDGE('',*,*,#9476,.T.);
#13263=ORIENTED_EDGE('',*,*,#9477,.F.);
#13264=ORIENTED_EDGE('',*,*,#9478,.F.);
#13265=ORIENTED_EDGE('',*,*,#9479,.T.);
#13266=ORIENTED_EDGE('',*,*,#9480,.F.);
#13267=ORIENTED_EDGE('',*,*,#9481,.T.);
#13268=ORIENTED_EDGE('',*,*,#9482,.F.);
#13269=ORIENTED_EDGE('',*,*,#9481,.F.);
#13270=ORIENTED_EDGE('',*,*,#9483,.F.);
#13271=ORIENTED_EDGE('',*,*,#9484,.F.);
#13272=ORIENTED_EDGE('',*,*,#9485,.T.);
#13273=ORIENTED_EDGE('',*,*,#9486,.F.);
#13274=ORIENTED_EDGE('',*,*,#9487,.F.);
#13275=ORIENTED_EDGE('',*,*,#9488,.T.);
#13276=ORIENTED_EDGE('',*,*,#9489,.F.);
#13277=ORIENTED_EDGE('',*,*,#9490,.F.);
#13278=ORIENTED_EDGE('',*,*,#9491,.T.);
#13279=ORIENTED_EDGE('',*,*,#9492,.F.);
#13280=ORIENTED_EDGE('',*,*,#9493,.F.);
#13281=ORIENTED_EDGE('',*,*,#9494,.T.);
#13282=ORIENTED_EDGE('',*,*,#9495,.F.);
#13283=ORIENTED_EDGE('',*,*,#9496,.F.);
#13284=ORIENTED_EDGE('',*,*,#9497,.T.);
#13285=ORIENTED_EDGE('',*,*,#9498,.F.);
#13286=ORIENTED_EDGE('',*,*,#9499,.F.);
#13287=ORIENTED_EDGE('',*,*,#9500,.T.);
#13288=ORIENTED_EDGE('',*,*,#9501,.F.);
#13289=ORIENTED_EDGE('',*,*,#9502,.F.);
#13290=ORIENTED_EDGE('',*,*,#9503,.T.);
#13291=ORIENTED_EDGE('',*,*,#9504,.F.);
#13292=ORIENTED_EDGE('',*,*,#9505,.F.);
#13293=ORIENTED_EDGE('',*,*,#9506,.T.);
#13294=ORIENTED_EDGE('',*,*,#9507,.F.);
#13295=ORIENTED_EDGE('',*,*,#9508,.F.);
#13296=ORIENTED_EDGE('',*,*,#9509,.T.);
#13297=ORIENTED_EDGE('',*,*,#9510,.F.);
#13298=ORIENTED_EDGE('',*,*,#9511,.F.);
#13299=ORIENTED_EDGE('',*,*,#9512,.T.);
#13300=ORIENTED_EDGE('',*,*,#9513,.F.);
#13301=ORIENTED_EDGE('',*,*,#9514,.F.);
#13302=ORIENTED_EDGE('',*,*,#9515,.T.);
#13303=ORIENTED_EDGE('',*,*,#9516,.F.);
#13304=ORIENTED_EDGE('',*,*,#9517,.F.);
#13305=ORIENTED_EDGE('',*,*,#9518,.T.);
#13306=ORIENTED_EDGE('',*,*,#9519,.F.);
#13307=ORIENTED_EDGE('',*,*,#9520,.F.);
#13308=ORIENTED_EDGE('',*,*,#9521,.T.);
#13309=ORIENTED_EDGE('',*,*,#9522,.F.);
#13310=ORIENTED_EDGE('',*,*,#9523,.F.);
#13311=ORIENTED_EDGE('',*,*,#9524,.T.);
#13312=ORIENTED_EDGE('',*,*,#9525,.F.);
#13313=ORIENTED_EDGE('',*,*,#9526,.F.);
#13314=ORIENTED_EDGE('',*,*,#9527,.T.);
#13315=ORIENTED_EDGE('',*,*,#9528,.F.);
#13316=ORIENTED_EDGE('',*,*,#9529,.F.);
#13317=ORIENTED_EDGE('',*,*,#9530,.T.);
#13318=ORIENTED_EDGE('',*,*,#9531,.F.);
#13319=ORIENTED_EDGE('',*,*,#9532,.F.);
#13320=ORIENTED_EDGE('',*,*,#9533,.T.);
#13321=ORIENTED_EDGE('',*,*,#9534,.F.);
#13322=ORIENTED_EDGE('',*,*,#9535,.F.);
#13323=ORIENTED_EDGE('',*,*,#9536,.T.);
#13324=ORIENTED_EDGE('',*,*,#9537,.F.);
#13325=ORIENTED_EDGE('',*,*,#9538,.F.);
#13326=ORIENTED_EDGE('',*,*,#9539,.T.);
#13327=ORIENTED_EDGE('',*,*,#9540,.F.);
#13328=ORIENTED_EDGE('',*,*,#9541,.F.);
#13329=ORIENTED_EDGE('',*,*,#9542,.T.);
#13330=ORIENTED_EDGE('',*,*,#9543,.F.);
#13331=ORIENTED_EDGE('',*,*,#9544,.F.);
#13332=ORIENTED_EDGE('',*,*,#9545,.T.);
#13333=ORIENTED_EDGE('',*,*,#9546,.F.);
#13334=ORIENTED_EDGE('',*,*,#9547,.F.);
#13335=ORIENTED_EDGE('',*,*,#9548,.T.);
#13336=ORIENTED_EDGE('',*,*,#9549,.F.);
#13337=ORIENTED_EDGE('',*,*,#9550,.F.);
#13338=ORIENTED_EDGE('',*,*,#9551,.T.);
#13339=ORIENTED_EDGE('',*,*,#9552,.F.);
#13340=ORIENTED_EDGE('',*,*,#9553,.F.);
#13341=ORIENTED_EDGE('',*,*,#9554,.T.);
#13342=ORIENTED_EDGE('',*,*,#9555,.F.);
#13343=ORIENTED_EDGE('',*,*,#9556,.F.);
#13344=ORIENTED_EDGE('',*,*,#9557,.T.);
#13345=ORIENTED_EDGE('',*,*,#9558,.F.);
#13346=ORIENTED_EDGE('',*,*,#9559,.F.);
#13347=ORIENTED_EDGE('',*,*,#9560,.T.);
#13348=ORIENTED_EDGE('',*,*,#9561,.F.);
#13349=ORIENTED_EDGE('',*,*,#9562,.F.);
#13350=ORIENTED_EDGE('',*,*,#9563,.T.);
#13351=ORIENTED_EDGE('',*,*,#9564,.F.);
#13352=ORIENTED_EDGE('',*,*,#9565,.F.);
#13353=ORIENTED_EDGE('',*,*,#9566,.T.);
#13354=ORIENTED_EDGE('',*,*,#9567,.F.);
#13355=ORIENTED_EDGE('',*,*,#9568,.F.);
#13356=ORIENTED_EDGE('',*,*,#9569,.T.);
#13357=ORIENTED_EDGE('',*,*,#9570,.F.);
#13358=ORIENTED_EDGE('',*,*,#9571,.F.);
#13359=ORIENTED_EDGE('',*,*,#9572,.T.);
#13360=ORIENTED_EDGE('',*,*,#9573,.F.);
#13361=ORIENTED_EDGE('',*,*,#9574,.F.);
#13362=ORIENTED_EDGE('',*,*,#9575,.T.);
#13363=ORIENTED_EDGE('',*,*,#9576,.F.);
#13364=ORIENTED_EDGE('',*,*,#9577,.F.);
#13365=ORIENTED_EDGE('',*,*,#9578,.T.);
#13366=ORIENTED_EDGE('',*,*,#9579,.F.);
#13367=ORIENTED_EDGE('',*,*,#9580,.F.);
#13368=ORIENTED_EDGE('',*,*,#9581,.T.);
#13369=ORIENTED_EDGE('',*,*,#9582,.F.);
#13370=ORIENTED_EDGE('',*,*,#9583,.F.);
#13371=ORIENTED_EDGE('',*,*,#9584,.T.);
#13372=ORIENTED_EDGE('',*,*,#9585,.F.);
#13373=ORIENTED_EDGE('',*,*,#9586,.F.);
#13374=ORIENTED_EDGE('',*,*,#9587,.T.);
#13375=ORIENTED_EDGE('',*,*,#9588,.F.);
#13376=ORIENTED_EDGE('',*,*,#9589,.F.);
#13377=ORIENTED_EDGE('',*,*,#9590,.T.);
#13378=ORIENTED_EDGE('',*,*,#9591,.F.);
#13379=ORIENTED_EDGE('',*,*,#9592,.F.);
#13380=ORIENTED_EDGE('',*,*,#9593,.T.);
#13381=ORIENTED_EDGE('',*,*,#9594,.F.);
#13382=ORIENTED_EDGE('',*,*,#9595,.F.);
#13383=ORIENTED_EDGE('',*,*,#9596,.T.);
#13384=ORIENTED_EDGE('',*,*,#9597,.F.);
#13385=ORIENTED_EDGE('',*,*,#9598,.T.);
#13386=ORIENTED_EDGE('',*,*,#9599,.F.);
#13387=ORIENTED_EDGE('',*,*,#9600,.T.);
#13388=ORIENTED_EDGE('',*,*,#9601,.T.);
#13389=ORIENTED_EDGE('',*,*,#9602,.F.);
#13390=ORIENTED_EDGE('',*,*,#9603,.T.);
#13391=ORIENTED_EDGE('',*,*,#9604,.T.);
#13392=ORIENTED_EDGE('',*,*,#9605,.F.);
#13393=ORIENTED_EDGE('',*,*,#9606,.T.);
#13394=ORIENTED_EDGE('',*,*,#9607,.T.);
#13395=ORIENTED_EDGE('',*,*,#9608,.F.);
#13396=ORIENTED_EDGE('',*,*,#9609,.T.);
#13397=ORIENTED_EDGE('',*,*,#9610,.T.);
#13398=ORIENTED_EDGE('',*,*,#9611,.F.);
#13399=ORIENTED_EDGE('',*,*,#9612,.T.);
#13400=ORIENTED_EDGE('',*,*,#9613,.T.);
#13401=ORIENTED_EDGE('',*,*,#9614,.F.);
#13402=ORIENTED_EDGE('',*,*,#9615,.T.);
#13403=ORIENTED_EDGE('',*,*,#9616,.T.);
#13404=ORIENTED_EDGE('',*,*,#9617,.F.);
#13405=ORIENTED_EDGE('',*,*,#9618,.T.);
#13406=ORIENTED_EDGE('',*,*,#9619,.T.);
#13407=ORIENTED_EDGE('',*,*,#9620,.F.);
#13408=ORIENTED_EDGE('',*,*,#9621,.T.);
#13409=ORIENTED_EDGE('',*,*,#9622,.T.);
#13410=ORIENTED_EDGE('',*,*,#9623,.F.);
#13411=ORIENTED_EDGE('',*,*,#9624,.T.);
#13412=ORIENTED_EDGE('',*,*,#9625,.T.);
#13413=ORIENTED_EDGE('',*,*,#9626,.F.);
#13414=ORIENTED_EDGE('',*,*,#9627,.T.);
#13415=ORIENTED_EDGE('',*,*,#9628,.T.);
#13416=ORIENTED_EDGE('',*,*,#9629,.F.);
#13417=ORIENTED_EDGE('',*,*,#9630,.T.);
#13418=ORIENTED_EDGE('',*,*,#9631,.T.);
#13419=ORIENTED_EDGE('',*,*,#9632,.F.);
#13420=ORIENTED_EDGE('',*,*,#9633,.T.);
#13421=ORIENTED_EDGE('',*,*,#9634,.T.);
#13422=ORIENTED_EDGE('',*,*,#9635,.F.);
#13423=ORIENTED_EDGE('',*,*,#9636,.T.);
#13424=ORIENTED_EDGE('',*,*,#9637,.T.);
#13425=ORIENTED_EDGE('',*,*,#9638,.F.);
#13426=ORIENTED_EDGE('',*,*,#9639,.T.);
#13427=ORIENTED_EDGE('',*,*,#9640,.T.);
#13428=ORIENTED_EDGE('',*,*,#9641,.F.);
#13429=ORIENTED_EDGE('',*,*,#9642,.T.);
#13430=ORIENTED_EDGE('',*,*,#9643,.T.);
#13431=ORIENTED_EDGE('',*,*,#9644,.F.);
#13432=ORIENTED_EDGE('',*,*,#9645,.T.);
#13433=ORIENTED_EDGE('',*,*,#9646,.T.);
#13434=ORIENTED_EDGE('',*,*,#9647,.F.);
#13435=ORIENTED_EDGE('',*,*,#9648,.T.);
#13436=ORIENTED_EDGE('',*,*,#9649,.T.);
#13437=ORIENTED_EDGE('',*,*,#9650,.F.);
#13438=ORIENTED_EDGE('',*,*,#9651,.T.);
#13439=ORIENTED_EDGE('',*,*,#9652,.T.);
#13440=ORIENTED_EDGE('',*,*,#9653,.F.);
#13441=ORIENTED_EDGE('',*,*,#9654,.T.);
#13442=ORIENTED_EDGE('',*,*,#9655,.T.);
#13443=ORIENTED_EDGE('',*,*,#9656,.F.);
#13444=ORIENTED_EDGE('',*,*,#9657,.T.);
#13445=ORIENTED_EDGE('',*,*,#9658,.T.);
#13446=ORIENTED_EDGE('',*,*,#9659,.F.);
#13447=ORIENTED_EDGE('',*,*,#9660,.T.);
#13448=ORIENTED_EDGE('',*,*,#9661,.T.);
#13449=ORIENTED_EDGE('',*,*,#9662,.F.);
#13450=ORIENTED_EDGE('',*,*,#9663,.T.);
#13451=ORIENTED_EDGE('',*,*,#9664,.T.);
#13452=ORIENTED_EDGE('',*,*,#9665,.F.);
#13453=ORIENTED_EDGE('',*,*,#9666,.T.);
#13454=ORIENTED_EDGE('',*,*,#9667,.T.);
#13455=ORIENTED_EDGE('',*,*,#9668,.F.);
#13456=ORIENTED_EDGE('',*,*,#9669,.T.);
#13457=ORIENTED_EDGE('',*,*,#9670,.T.);
#13458=ORIENTED_EDGE('',*,*,#9671,.F.);
#13459=ORIENTED_EDGE('',*,*,#9672,.T.);
#13460=ORIENTED_EDGE('',*,*,#9673,.T.);
#13461=ORIENTED_EDGE('',*,*,#9674,.F.);
#13462=ORIENTED_EDGE('',*,*,#9675,.T.);
#13463=ORIENTED_EDGE('',*,*,#9676,.T.);
#13464=ORIENTED_EDGE('',*,*,#9677,.F.);
#13465=ORIENTED_EDGE('',*,*,#9678,.T.);
#13466=ORIENTED_EDGE('',*,*,#9679,.T.);
#13467=ORIENTED_EDGE('',*,*,#9680,.F.);
#13468=ORIENTED_EDGE('',*,*,#9681,.T.);
#13469=ORIENTED_EDGE('',*,*,#9682,.T.);
#13470=ORIENTED_EDGE('',*,*,#9683,.F.);
#13471=ORIENTED_EDGE('',*,*,#9684,.T.);
#13472=ORIENTED_EDGE('',*,*,#9685,.T.);
#13473=ORIENTED_EDGE('',*,*,#9686,.F.);
#13474=ORIENTED_EDGE('',*,*,#9687,.T.);
#13475=ORIENTED_EDGE('',*,*,#9688,.T.);
#13476=ORIENTED_EDGE('',*,*,#9689,.F.);
#13477=ORIENTED_EDGE('',*,*,#9690,.T.);
#13478=ORIENTED_EDGE('',*,*,#9691,.T.);
#13479=ORIENTED_EDGE('',*,*,#9692,.F.);
#13480=ORIENTED_EDGE('',*,*,#9693,.T.);
#13481=ORIENTED_EDGE('',*,*,#9694,.T.);
#13482=ORIENTED_EDGE('',*,*,#9695,.F.);
#13483=ORIENTED_EDGE('',*,*,#9696,.T.);
#13484=ORIENTED_EDGE('',*,*,#9697,.T.);
#13485=ORIENTED_EDGE('',*,*,#9698,.F.);
#13486=ORIENTED_EDGE('',*,*,#9699,.T.);
#13487=ORIENTED_EDGE('',*,*,#9700,.T.);
#13488=ORIENTED_EDGE('',*,*,#9701,.F.);
#13489=ORIENTED_EDGE('',*,*,#9702,.T.);
#13490=ORIENTED_EDGE('',*,*,#9703,.T.);
#13491=ORIENTED_EDGE('',*,*,#9704,.F.);
#13492=ORIENTED_EDGE('',*,*,#9705,.T.);
#13493=ORIENTED_EDGE('',*,*,#9706,.T.);
#13494=ORIENTED_EDGE('',*,*,#9707,.F.);
#13495=ORIENTED_EDGE('',*,*,#9708,.T.);
#13496=ORIENTED_EDGE('',*,*,#9709,.T.);
#13497=ORIENTED_EDGE('',*,*,#9710,.F.);
#13498=ORIENTED_EDGE('',*,*,#9711,.T.);
#13499=ORIENTED_EDGE('',*,*,#9712,.T.);
#13500=ORIENTED_EDGE('',*,*,#9713,.F.);
#13501=ORIENTED_EDGE('',*,*,#9714,.T.);
#13502=ORIENTED_EDGE('',*,*,#9715,.T.);
#13503=ORIENTED_EDGE('',*,*,#9716,.T.);
#13504=ORIENTED_EDGE('',*,*,#9715,.F.);
#13505=ORIENTED_EDGE('',*,*,#9717,.T.);
#13506=ORIENTED_EDGE('',*,*,#9718,.T.);
#13507=ORIENTED_EDGE('',*,*,#9719,.F.);
#13508=ORIENTED_EDGE('',*,*,#9720,.T.);
#13509=ORIENTED_EDGE('',*,*,#9721,.T.);
#13510=ORIENTED_EDGE('',*,*,#9722,.F.);
#13511=ORIENTED_EDGE('',*,*,#9723,.T.);
#13512=ORIENTED_EDGE('',*,*,#9724,.T.);
#13513=ORIENTED_EDGE('',*,*,#9725,.F.);
#13514=ORIENTED_EDGE('',*,*,#9726,.T.);
#13515=ORIENTED_EDGE('',*,*,#9727,.T.);
#13516=ORIENTED_EDGE('',*,*,#9728,.F.);
#13517=ORIENTED_EDGE('',*,*,#9729,.T.);
#13518=ORIENTED_EDGE('',*,*,#9730,.T.);
#13519=ORIENTED_EDGE('',*,*,#9731,.F.);
#13520=ORIENTED_EDGE('',*,*,#9732,.T.);
#13521=ORIENTED_EDGE('',*,*,#9733,.T.);
#13522=ORIENTED_EDGE('',*,*,#9734,.F.);
#13523=ORIENTED_EDGE('',*,*,#9735,.T.);
#13524=ORIENTED_EDGE('',*,*,#9736,.T.);
#13525=ORIENTED_EDGE('',*,*,#9737,.F.);
#13526=ORIENTED_EDGE('',*,*,#9738,.T.);
#13527=ORIENTED_EDGE('',*,*,#9739,.T.);
#13528=ORIENTED_EDGE('',*,*,#9740,.F.);
#13529=ORIENTED_EDGE('',*,*,#9741,.T.);
#13530=ORIENTED_EDGE('',*,*,#9742,.T.);
#13531=ORIENTED_EDGE('',*,*,#9743,.F.);
#13532=ORIENTED_EDGE('',*,*,#9744,.T.);
#13533=ORIENTED_EDGE('',*,*,#9745,.T.);
#13534=ORIENTED_EDGE('',*,*,#9746,.F.);
#13535=ORIENTED_EDGE('',*,*,#9747,.T.);
#13536=ORIENTED_EDGE('',*,*,#9748,.T.);
#13537=ORIENTED_EDGE('',*,*,#9749,.F.);
#13538=ORIENTED_EDGE('',*,*,#9750,.T.);
#13539=ORIENTED_EDGE('',*,*,#9751,.T.);
#13540=ORIENTED_EDGE('',*,*,#9752,.F.);
#13541=ORIENTED_EDGE('',*,*,#9753,.T.);
#13542=ORIENTED_EDGE('',*,*,#9754,.T.);
#13543=ORIENTED_EDGE('',*,*,#9755,.F.);
#13544=ORIENTED_EDGE('',*,*,#9756,.T.);
#13545=ORIENTED_EDGE('',*,*,#9757,.T.);
#13546=ORIENTED_EDGE('',*,*,#9758,.F.);
#13547=ORIENTED_EDGE('',*,*,#9759,.T.);
#13548=ORIENTED_EDGE('',*,*,#9760,.T.);
#13549=ORIENTED_EDGE('',*,*,#9761,.F.);
#13550=ORIENTED_EDGE('',*,*,#9762,.T.);
#13551=ORIENTED_EDGE('',*,*,#9763,.T.);
#13552=ORIENTED_EDGE('',*,*,#9764,.F.);
#13553=ORIENTED_EDGE('',*,*,#9765,.T.);
#13554=ORIENTED_EDGE('',*,*,#9766,.T.);
#13555=ORIENTED_EDGE('',*,*,#9767,.F.);
#13556=ORIENTED_EDGE('',*,*,#9768,.T.);
#13557=ORIENTED_EDGE('',*,*,#9769,.T.);
#13558=ORIENTED_EDGE('',*,*,#9770,.F.);
#13559=ORIENTED_EDGE('',*,*,#9771,.T.);
#13560=ORIENTED_EDGE('',*,*,#9772,.T.);
#13561=ORIENTED_EDGE('',*,*,#9773,.F.);
#13562=ORIENTED_EDGE('',*,*,#9774,.T.);
#13563=ORIENTED_EDGE('',*,*,#9775,.T.);
#13564=ORIENTED_EDGE('',*,*,#9776,.F.);
#13565=ORIENTED_EDGE('',*,*,#9777,.T.);
#13566=ORIENTED_EDGE('',*,*,#9778,.T.);
#13567=ORIENTED_EDGE('',*,*,#9779,.F.);
#13568=ORIENTED_EDGE('',*,*,#9780,.T.);
#13569=ORIENTED_EDGE('',*,*,#9781,.T.);
#13570=ORIENTED_EDGE('',*,*,#9782,.F.);
#13571=ORIENTED_EDGE('',*,*,#9783,.T.);
#13572=ORIENTED_EDGE('',*,*,#9784,.T.);
#13573=ORIENTED_EDGE('',*,*,#9785,.F.);
#13574=ORIENTED_EDGE('',*,*,#9786,.T.);
#13575=ORIENTED_EDGE('',*,*,#9787,.T.);
#13576=ORIENTED_EDGE('',*,*,#9788,.F.);
#13577=ORIENTED_EDGE('',*,*,#9789,.T.);
#13578=ORIENTED_EDGE('',*,*,#9790,.T.);
#13579=ORIENTED_EDGE('',*,*,#9791,.F.);
#13580=ORIENTED_EDGE('',*,*,#9792,.T.);
#13581=ORIENTED_EDGE('',*,*,#9793,.T.);
#13582=ORIENTED_EDGE('',*,*,#9794,.F.);
#13583=ORIENTED_EDGE('',*,*,#9795,.T.);
#13584=ORIENTED_EDGE('',*,*,#9796,.T.);
#13585=ORIENTED_EDGE('',*,*,#9797,.F.);
#13586=ORIENTED_EDGE('',*,*,#9798,.T.);
#13587=ORIENTED_EDGE('',*,*,#9799,.T.);
#13588=ORIENTED_EDGE('',*,*,#9800,.F.);
#13589=ORIENTED_EDGE('',*,*,#9801,.T.);
#13590=ORIENTED_EDGE('',*,*,#9802,.T.);
#13591=ORIENTED_EDGE('',*,*,#9803,.F.);
#13592=ORIENTED_EDGE('',*,*,#9804,.T.);
#13593=ORIENTED_EDGE('',*,*,#9805,.T.);
#13594=ORIENTED_EDGE('',*,*,#9806,.F.);
#13595=ORIENTED_EDGE('',*,*,#9807,.T.);
#13596=ORIENTED_EDGE('',*,*,#9808,.T.);
#13597=ORIENTED_EDGE('',*,*,#9809,.F.);
#13598=ORIENTED_EDGE('',*,*,#9810,.T.);
#13599=ORIENTED_EDGE('',*,*,#9811,.T.);
#13600=ORIENTED_EDGE('',*,*,#9812,.F.);
#13601=ORIENTED_EDGE('',*,*,#9813,.T.);
#13602=ORIENTED_EDGE('',*,*,#9814,.T.);
#13603=ORIENTED_EDGE('',*,*,#9815,.F.);
#13604=ORIENTED_EDGE('',*,*,#9816,.T.);
#13605=ORIENTED_EDGE('',*,*,#9817,.T.);
#13606=ORIENTED_EDGE('',*,*,#9818,.F.);
#13607=ORIENTED_EDGE('',*,*,#9819,.T.);
#13608=ORIENTED_EDGE('',*,*,#9820,.T.);
#13609=ORIENTED_EDGE('',*,*,#9821,.F.);
#13610=ORIENTED_EDGE('',*,*,#9822,.T.);
#13611=ORIENTED_EDGE('',*,*,#9823,.T.);
#13612=ORIENTED_EDGE('',*,*,#9824,.F.);
#13613=ORIENTED_EDGE('',*,*,#9825,.T.);
#13614=ORIENTED_EDGE('',*,*,#9826,.T.);
#13615=ORIENTED_EDGE('',*,*,#9827,.F.);
#13616=ORIENTED_EDGE('',*,*,#9828,.T.);
#13617=ORIENTED_EDGE('',*,*,#9829,.T.);
#13618=ORIENTED_EDGE('',*,*,#9830,.F.);
#13619=ORIENTED_EDGE('',*,*,#9831,.T.);
#13620=ORIENTED_EDGE('',*,*,#9227,.T.);
#13621=ORIENTED_EDGE('',*,*,#9832,.T.);
#13622=ORIENTED_EDGE('',*,*,#9358,.T.);
#13623=ORIENTED_EDGE('',*,*,#9359,.T.);
#13624=ORIENTED_EDGE('',*,*,#9832,.F.);
#13625=ORIENTED_EDGE('',*,*,#9833,.F.);
#13626=ORIENTED_EDGE('',*,*,#9779,.T.);
#13627=ORIENTED_EDGE('',*,*,#9834,.T.);
#13628=ORIENTED_EDGE('',*,*,#9536,.F.);
#13629=ORIENTED_EDGE('',*,*,#9835,.T.);
#13630=ORIENTED_EDGE('',*,*,#9533,.F.);
#13631=ORIENTED_EDGE('',*,*,#9836,.F.);
#13632=ORIENTED_EDGE('',*,*,#9782,.T.);
#13633=ORIENTED_EDGE('',*,*,#9837,.T.);
#13634=ORIENTED_EDGE('',*,*,#9530,.F.);
#13635=ORIENTED_EDGE('',*,*,#9838,.F.);
#13636=ORIENTED_EDGE('',*,*,#9785,.T.);
#13637=ORIENTED_EDGE('',*,*,#9839,.T.);
#13638=ORIENTED_EDGE('',*,*,#9527,.F.);
#13639=ORIENTED_EDGE('',*,*,#9840,.F.);
#13640=ORIENTED_EDGE('',*,*,#9788,.T.);
#13641=ORIENTED_EDGE('',*,*,#9841,.T.);
#13642=ORIENTED_EDGE('',*,*,#9524,.F.);
#13643=ORIENTED_EDGE('',*,*,#9842,.F.);
#13644=ORIENTED_EDGE('',*,*,#9791,.T.);
#13645=ORIENTED_EDGE('',*,*,#9843,.T.);
#13646=ORIENTED_EDGE('',*,*,#9521,.F.);
#13647=ORIENTED_EDGE('',*,*,#9844,.F.);
#13648=ORIENTED_EDGE('',*,*,#9794,.T.);
#13649=ORIENTED_EDGE('',*,*,#9845,.T.);
#13650=ORIENTED_EDGE('',*,*,#9518,.F.);
#13651=ORIENTED_EDGE('',*,*,#9846,.F.);
#13652=ORIENTED_EDGE('',*,*,#9797,.T.);
#13653=ORIENTED_EDGE('',*,*,#9847,.T.);
#13654=ORIENTED_EDGE('',*,*,#9515,.F.);
#13655=ORIENTED_EDGE('',*,*,#9848,.F.);
#13656=ORIENTED_EDGE('',*,*,#9800,.T.);
#13657=ORIENTED_EDGE('',*,*,#9849,.T.);
#13658=ORIENTED_EDGE('',*,*,#9512,.F.);
#13659=ORIENTED_EDGE('',*,*,#9850,.F.);
#13660=ORIENTED_EDGE('',*,*,#9803,.T.);
#13661=ORIENTED_EDGE('',*,*,#9851,.T.);
#13662=ORIENTED_EDGE('',*,*,#9509,.F.);
#13663=ORIENTED_EDGE('',*,*,#9852,.F.);
#13664=ORIENTED_EDGE('',*,*,#9806,.T.);
#13665=ORIENTED_EDGE('',*,*,#9853,.T.);
#13666=ORIENTED_EDGE('',*,*,#9506,.F.);
#13667=ORIENTED_EDGE('',*,*,#9854,.F.);
#13668=ORIENTED_EDGE('',*,*,#9809,.T.);
#13669=ORIENTED_EDGE('',*,*,#9855,.T.);
#13670=ORIENTED_EDGE('',*,*,#9503,.F.);
#13671=ORIENTED_EDGE('',*,*,#9856,.F.);
#13672=ORIENTED_EDGE('',*,*,#9812,.T.);
#13673=ORIENTED_EDGE('',*,*,#9857,.T.);
#13674=ORIENTED_EDGE('',*,*,#9500,.F.);
#13675=ORIENTED_EDGE('',*,*,#9858,.F.);
#13676=ORIENTED_EDGE('',*,*,#9815,.T.);
#13677=ORIENTED_EDGE('',*,*,#9859,.T.);
#13678=ORIENTED_EDGE('',*,*,#9497,.F.);
#13679=ORIENTED_EDGE('',*,*,#9860,.F.);
#13680=ORIENTED_EDGE('',*,*,#9818,.T.);
#13681=ORIENTED_EDGE('',*,*,#9861,.T.);
#13682=ORIENTED_EDGE('',*,*,#9494,.F.);
#13683=ORIENTED_EDGE('',*,*,#9862,.F.);
#13684=ORIENTED_EDGE('',*,*,#9821,.T.);
#13685=ORIENTED_EDGE('',*,*,#9863,.T.);
#13686=ORIENTED_EDGE('',*,*,#9491,.F.);
#13687=ORIENTED_EDGE('',*,*,#9864,.F.);
#13688=ORIENTED_EDGE('',*,*,#9824,.T.);
#13689=ORIENTED_EDGE('',*,*,#9865,.T.);
#13690=ORIENTED_EDGE('',*,*,#9488,.F.);
#13691=ORIENTED_EDGE('',*,*,#9866,.F.);
#13692=ORIENTED_EDGE('',*,*,#9827,.T.);
#13693=ORIENTED_EDGE('',*,*,#9867,.T.);
#13694=ORIENTED_EDGE('',*,*,#9485,.F.);
#13695=ORIENTED_EDGE('',*,*,#9868,.F.);
#13696=ORIENTED_EDGE('',*,*,#9830,.T.);
#13697=ORIENTED_EDGE('',*,*,#9869,.T.);
#13698=ORIENTED_EDGE('',*,*,#9479,.F.);
#13699=ORIENTED_EDGE('',*,*,#9870,.F.);
#13700=ORIENTED_EDGE('',*,*,#9599,.T.);
#13701=ORIENTED_EDGE('',*,*,#9871,.T.);
#13702=ORIENTED_EDGE('',*,*,#9476,.F.);
#13703=ORIENTED_EDGE('',*,*,#9872,.F.);
#13704=ORIENTED_EDGE('',*,*,#9602,.T.);
#13705=ORIENTED_EDGE('',*,*,#9873,.T.);
#13706=ORIENTED_EDGE('',*,*,#9473,.F.);
#13707=ORIENTED_EDGE('',*,*,#9874,.F.);
#13708=ORIENTED_EDGE('',*,*,#9605,.T.);
#13709=ORIENTED_EDGE('',*,*,#9875,.T.);
#13710=ORIENTED_EDGE('',*,*,#9470,.F.);
#13711=ORIENTED_EDGE('',*,*,#9876,.F.);
#13712=ORIENTED_EDGE('',*,*,#9608,.T.);
#13713=ORIENTED_EDGE('',*,*,#9877,.T.);
#13714=ORIENTED_EDGE('',*,*,#9467,.F.);
#13715=ORIENTED_EDGE('',*,*,#9878,.F.);
#13716=ORIENTED_EDGE('',*,*,#9611,.T.);
#13717=ORIENTED_EDGE('',*,*,#9879,.T.);
#13718=ORIENTED_EDGE('',*,*,#9464,.F.);
#13719=ORIENTED_EDGE('',*,*,#9880,.F.);
#13720=ORIENTED_EDGE('',*,*,#9614,.T.);
#13721=ORIENTED_EDGE('',*,*,#9881,.T.);
#13722=ORIENTED_EDGE('',*,*,#9461,.F.);
#13723=ORIENTED_EDGE('',*,*,#9882,.F.);
#13724=ORIENTED_EDGE('',*,*,#9617,.T.);
#13725=ORIENTED_EDGE('',*,*,#9883,.T.);
#13726=ORIENTED_EDGE('',*,*,#9458,.F.);
#13727=ORIENTED_EDGE('',*,*,#9884,.F.);
#13728=ORIENTED_EDGE('',*,*,#9620,.T.);
#13729=ORIENTED_EDGE('',*,*,#9885,.T.);
#13730=ORIENTED_EDGE('',*,*,#9455,.F.);
#13731=ORIENTED_EDGE('',*,*,#9886,.F.);
#13732=ORIENTED_EDGE('',*,*,#9623,.T.);
#13733=ORIENTED_EDGE('',*,*,#9887,.T.);
#13734=ORIENTED_EDGE('',*,*,#9452,.F.);
#13735=ORIENTED_EDGE('',*,*,#9888,.F.);
#13736=ORIENTED_EDGE('',*,*,#9626,.T.);
#13737=ORIENTED_EDGE('',*,*,#9889,.T.);
#13738=ORIENTED_EDGE('',*,*,#9449,.F.);
#13739=ORIENTED_EDGE('',*,*,#9890,.F.);
#13740=ORIENTED_EDGE('',*,*,#9629,.T.);
#13741=ORIENTED_EDGE('',*,*,#9891,.T.);
#13742=ORIENTED_EDGE('',*,*,#9446,.F.);
#13743=ORIENTED_EDGE('',*,*,#9892,.F.);
#13744=ORIENTED_EDGE('',*,*,#9632,.T.);
#13745=ORIENTED_EDGE('',*,*,#9893,.T.);
#13746=ORIENTED_EDGE('',*,*,#9443,.F.);
#13747=ORIENTED_EDGE('',*,*,#9894,.F.);
#13748=ORIENTED_EDGE('',*,*,#9635,.T.);
#13749=ORIENTED_EDGE('',*,*,#9895,.T.);
#13750=ORIENTED_EDGE('',*,*,#9440,.F.);
#13751=ORIENTED_EDGE('',*,*,#9896,.F.);
#13752=ORIENTED_EDGE('',*,*,#9638,.T.);
#13753=ORIENTED_EDGE('',*,*,#9897,.T.);
#13754=ORIENTED_EDGE('',*,*,#9437,.F.);
#13755=ORIENTED_EDGE('',*,*,#9898,.F.);
#13756=ORIENTED_EDGE('',*,*,#9641,.T.);
#13757=ORIENTED_EDGE('',*,*,#9899,.T.);
#13758=ORIENTED_EDGE('',*,*,#9434,.F.);
#13759=ORIENTED_EDGE('',*,*,#9900,.F.);
#13760=ORIENTED_EDGE('',*,*,#9644,.T.);
#13761=ORIENTED_EDGE('',*,*,#9901,.T.);
#13762=ORIENTED_EDGE('',*,*,#9431,.F.);
#13763=ORIENTED_EDGE('',*,*,#9902,.F.);
#13764=ORIENTED_EDGE('',*,*,#9647,.T.);
#13765=ORIENTED_EDGE('',*,*,#9903,.T.);
#13766=ORIENTED_EDGE('',*,*,#9428,.F.);
#13767=ORIENTED_EDGE('',*,*,#9904,.F.);
#13768=ORIENTED_EDGE('',*,*,#9650,.T.);
#13769=ORIENTED_EDGE('',*,*,#9905,.T.);
#13770=ORIENTED_EDGE('',*,*,#9425,.F.);
#13771=ORIENTED_EDGE('',*,*,#9906,.F.);
#13772=ORIENTED_EDGE('',*,*,#9653,.T.);
#13773=ORIENTED_EDGE('',*,*,#9907,.T.);
#13774=ORIENTED_EDGE('',*,*,#9422,.F.);
#13775=ORIENTED_EDGE('',*,*,#9908,.F.);
#13776=ORIENTED_EDGE('',*,*,#9656,.T.);
#13777=ORIENTED_EDGE('',*,*,#9909,.T.);
#13778=ORIENTED_EDGE('',*,*,#9419,.F.);
#13779=ORIENTED_EDGE('',*,*,#9910,.F.);
#13780=ORIENTED_EDGE('',*,*,#9659,.T.);
#13781=ORIENTED_EDGE('',*,*,#9911,.T.);
#13782=ORIENTED_EDGE('',*,*,#9416,.F.);
#13783=ORIENTED_EDGE('',*,*,#9912,.F.);
#13784=ORIENTED_EDGE('',*,*,#9662,.T.);
#13785=ORIENTED_EDGE('',*,*,#9913,.T.);
#13786=ORIENTED_EDGE('',*,*,#9413,.F.);
#13787=ORIENTED_EDGE('',*,*,#9914,.F.);
#13788=ORIENTED_EDGE('',*,*,#9665,.T.);
#13789=ORIENTED_EDGE('',*,*,#9915,.T.);
#13790=ORIENTED_EDGE('',*,*,#9410,.F.);
#13791=ORIENTED_EDGE('',*,*,#9916,.F.);
#13792=ORIENTED_EDGE('',*,*,#9668,.T.);
#13793=ORIENTED_EDGE('',*,*,#9917,.T.);
#13794=ORIENTED_EDGE('',*,*,#9407,.F.);
#13795=ORIENTED_EDGE('',*,*,#9918,.F.);
#13796=ORIENTED_EDGE('',*,*,#9671,.T.);
#13797=ORIENTED_EDGE('',*,*,#9919,.T.);
#13798=ORIENTED_EDGE('',*,*,#9404,.F.);
#13799=ORIENTED_EDGE('',*,*,#9920,.F.);
#13800=ORIENTED_EDGE('',*,*,#9674,.T.);
#13801=ORIENTED_EDGE('',*,*,#9921,.T.);
#13802=ORIENTED_EDGE('',*,*,#9401,.F.);
#13803=ORIENTED_EDGE('',*,*,#9922,.F.);
#13804=ORIENTED_EDGE('',*,*,#9677,.T.);
#13805=ORIENTED_EDGE('',*,*,#9923,.T.);
#13806=ORIENTED_EDGE('',*,*,#9398,.F.);
#13807=ORIENTED_EDGE('',*,*,#9924,.F.);
#13808=ORIENTED_EDGE('',*,*,#9680,.T.);
#13809=ORIENTED_EDGE('',*,*,#9925,.T.);
#13810=ORIENTED_EDGE('',*,*,#9395,.F.);
#13811=ORIENTED_EDGE('',*,*,#9926,.F.);
#13812=ORIENTED_EDGE('',*,*,#9683,.T.);
#13813=ORIENTED_EDGE('',*,*,#9927,.T.);
#13814=ORIENTED_EDGE('',*,*,#9392,.F.);
#13815=ORIENTED_EDGE('',*,*,#9928,.F.);
#13816=ORIENTED_EDGE('',*,*,#9686,.T.);
#13817=ORIENTED_EDGE('',*,*,#9929,.T.);
#13818=ORIENTED_EDGE('',*,*,#9389,.F.);
#13819=ORIENTED_EDGE('',*,*,#9930,.F.);
#13820=ORIENTED_EDGE('',*,*,#9689,.T.);
#13821=ORIENTED_EDGE('',*,*,#9931,.T.);
#13822=ORIENTED_EDGE('',*,*,#9386,.F.);
#13823=ORIENTED_EDGE('',*,*,#9932,.F.);
#13824=ORIENTED_EDGE('',*,*,#9692,.T.);
#13825=ORIENTED_EDGE('',*,*,#9933,.T.);
#13826=ORIENTED_EDGE('',*,*,#9383,.F.);
#13827=ORIENTED_EDGE('',*,*,#9934,.F.);
#13828=ORIENTED_EDGE('',*,*,#9695,.T.);
#13829=ORIENTED_EDGE('',*,*,#9935,.T.);
#13830=ORIENTED_EDGE('',*,*,#9380,.F.);
#13831=ORIENTED_EDGE('',*,*,#9936,.F.);
#13832=ORIENTED_EDGE('',*,*,#9698,.T.);
#13833=ORIENTED_EDGE('',*,*,#9937,.T.);
#13834=ORIENTED_EDGE('',*,*,#9377,.F.);
#13835=ORIENTED_EDGE('',*,*,#9938,.F.);
#13836=ORIENTED_EDGE('',*,*,#9701,.T.);
#13837=ORIENTED_EDGE('',*,*,#9939,.T.);
#13838=ORIENTED_EDGE('',*,*,#9374,.F.);
#13839=ORIENTED_EDGE('',*,*,#9940,.F.);
#13840=ORIENTED_EDGE('',*,*,#9704,.T.);
#13841=ORIENTED_EDGE('',*,*,#9941,.T.);
#13842=ORIENTED_EDGE('',*,*,#9371,.F.);
#13843=ORIENTED_EDGE('',*,*,#9942,.F.);
#13844=ORIENTED_EDGE('',*,*,#9707,.T.);
#13845=ORIENTED_EDGE('',*,*,#9943,.T.);
#13846=ORIENTED_EDGE('',*,*,#9368,.F.);
#13847=ORIENTED_EDGE('',*,*,#9944,.F.);
#13848=ORIENTED_EDGE('',*,*,#9710,.T.);
#13849=ORIENTED_EDGE('',*,*,#9945,.T.);
#13850=ORIENTED_EDGE('',*,*,#9365,.F.);
#13851=ORIENTED_EDGE('',*,*,#9946,.F.);
#13852=ORIENTED_EDGE('',*,*,#9713,.T.);
#13853=ORIENTED_EDGE('',*,*,#9947,.T.);
#13854=ORIENTED_EDGE('',*,*,#9596,.F.);
#13855=ORIENTED_EDGE('',*,*,#9948,.F.);
#13856=ORIENTED_EDGE('',*,*,#9719,.T.);
#13857=ORIENTED_EDGE('',*,*,#9949,.T.);
#13858=ORIENTED_EDGE('',*,*,#9593,.F.);
#13859=ORIENTED_EDGE('',*,*,#9950,.F.);
#13860=ORIENTED_EDGE('',*,*,#9722,.T.);
#13861=ORIENTED_EDGE('',*,*,#9951,.T.);
#13862=ORIENTED_EDGE('',*,*,#9590,.F.);
#13863=ORIENTED_EDGE('',*,*,#9952,.F.);
#13864=ORIENTED_EDGE('',*,*,#9725,.T.);
#13865=ORIENTED_EDGE('',*,*,#9953,.T.);
#13866=ORIENTED_EDGE('',*,*,#9587,.F.);
#13867=ORIENTED_EDGE('',*,*,#9954,.F.);
#13868=ORIENTED_EDGE('',*,*,#9728,.T.);
#13869=ORIENTED_EDGE('',*,*,#9955,.T.);
#13870=ORIENTED_EDGE('',*,*,#9584,.F.);
#13871=ORIENTED_EDGE('',*,*,#9956,.F.);
#13872=ORIENTED_EDGE('',*,*,#9731,.T.);
#13873=ORIENTED_EDGE('',*,*,#9957,.T.);
#13874=ORIENTED_EDGE('',*,*,#9581,.F.);
#13875=ORIENTED_EDGE('',*,*,#9958,.F.);
#13876=ORIENTED_EDGE('',*,*,#9734,.T.);
#13877=ORIENTED_EDGE('',*,*,#9959,.T.);
#13878=ORIENTED_EDGE('',*,*,#9578,.F.);
#13879=ORIENTED_EDGE('',*,*,#9960,.F.);
#13880=ORIENTED_EDGE('',*,*,#9737,.T.);
#13881=ORIENTED_EDGE('',*,*,#9961,.T.);
#13882=ORIENTED_EDGE('',*,*,#9575,.F.);
#13883=ORIENTED_EDGE('',*,*,#9962,.F.);
#13884=ORIENTED_EDGE('',*,*,#9740,.T.);
#13885=ORIENTED_EDGE('',*,*,#9963,.T.);
#13886=ORIENTED_EDGE('',*,*,#9572,.F.);
#13887=ORIENTED_EDGE('',*,*,#9964,.F.);
#13888=ORIENTED_EDGE('',*,*,#9743,.T.);
#13889=ORIENTED_EDGE('',*,*,#9965,.T.);
#13890=ORIENTED_EDGE('',*,*,#9569,.F.);
#13891=ORIENTED_EDGE('',*,*,#9966,.F.);
#13892=ORIENTED_EDGE('',*,*,#9746,.T.);
#13893=ORIENTED_EDGE('',*,*,#9967,.T.);
#13894=ORIENTED_EDGE('',*,*,#9566,.F.);
#13895=ORIENTED_EDGE('',*,*,#9968,.F.);
#13896=ORIENTED_EDGE('',*,*,#9749,.T.);
#13897=ORIENTED_EDGE('',*,*,#9969,.T.);
#13898=ORIENTED_EDGE('',*,*,#9563,.F.);
#13899=ORIENTED_EDGE('',*,*,#9970,.F.);
#13900=ORIENTED_EDGE('',*,*,#9752,.T.);
#13901=ORIENTED_EDGE('',*,*,#9971,.T.);
#13902=ORIENTED_EDGE('',*,*,#9560,.F.);
#13903=ORIENTED_EDGE('',*,*,#9972,.F.);
#13904=ORIENTED_EDGE('',*,*,#9755,.T.);
#13905=ORIENTED_EDGE('',*,*,#9973,.T.);
#13906=ORIENTED_EDGE('',*,*,#9557,.F.);
#13907=ORIENTED_EDGE('',*,*,#9974,.F.);
#13908=ORIENTED_EDGE('',*,*,#9758,.T.);
#13909=ORIENTED_EDGE('',*,*,#9975,.T.);
#13910=ORIENTED_EDGE('',*,*,#9554,.F.);
#13911=ORIENTED_EDGE('',*,*,#9976,.F.);
#13912=ORIENTED_EDGE('',*,*,#9761,.T.);
#13913=ORIENTED_EDGE('',*,*,#9977,.T.);
#13914=ORIENTED_EDGE('',*,*,#9551,.F.);
#13915=ORIENTED_EDGE('',*,*,#9978,.F.);
#13916=ORIENTED_EDGE('',*,*,#9764,.T.);
#13917=ORIENTED_EDGE('',*,*,#9979,.T.);
#13918=ORIENTED_EDGE('',*,*,#9548,.F.);
#13919=ORIENTED_EDGE('',*,*,#9980,.F.);
#13920=ORIENTED_EDGE('',*,*,#9767,.T.);
#13921=ORIENTED_EDGE('',*,*,#9981,.T.);
#13922=ORIENTED_EDGE('',*,*,#9545,.F.);
#13923=ORIENTED_EDGE('',*,*,#9982,.F.);
#13924=ORIENTED_EDGE('',*,*,#9770,.T.);
#13925=ORIENTED_EDGE('',*,*,#9983,.F.);
#13926=ORIENTED_EDGE('',*,*,#9776,.T.);
#13927=ORIENTED_EDGE('',*,*,#9984,.T.);
#13928=ORIENTED_EDGE('',*,*,#9539,.F.);
#13929=ORIENTED_EDGE('',*,*,#9716,.F.);
#13930=ORIENTED_EDGE('',*,*,#9225,.T.);
#13931=ORIENTED_EDGE('',*,*,#9985,.T.);
#13932=ORIENTED_EDGE('',*,*,#9542,.F.);
#13933=ORIENTED_EDGE('',*,*,#9986,.F.);
#13934=ORIENTED_EDGE('',*,*,#9773,.T.);
#13935=ORIENTED_EDGE('',*,*,#9482,.T.);
#13936=ORIENTED_EDGE('',*,*,#9231,.F.);
#13937=ORIENTED_EDGE('',*,*,#9986,.T.);
#13938=ORIENTED_EDGE('',*,*,#9541,.T.);
#13939=ORIENTED_EDGE('',*,*,#9987,.F.);
#13940=ORIENTED_EDGE('',*,*,#9774,.F.);
#13941=ORIENTED_EDGE('',*,*,#9987,.T.);
#13942=ORIENTED_EDGE('',*,*,#9540,.T.);
#13943=ORIENTED_EDGE('',*,*,#9984,.F.);
#13944=ORIENTED_EDGE('',*,*,#9775,.F.);
#13945=ORIENTED_EDGE('',*,*,#9983,.T.);
#13946=ORIENTED_EDGE('',*,*,#9538,.T.);
#13947=ORIENTED_EDGE('',*,*,#9988,.F.);
#13948=ORIENTED_EDGE('',*,*,#9777,.F.);
#13949=ORIENTED_EDGE('',*,*,#9988,.T.);
#13950=ORIENTED_EDGE('',*,*,#9537,.T.);
#13951=ORIENTED_EDGE('',*,*,#9834,.F.);
#13952=ORIENTED_EDGE('',*,*,#9778,.F.);
#13953=ORIENTED_EDGE('',*,*,#9982,.T.);
#13954=ORIENTED_EDGE('',*,*,#9544,.T.);
#13955=ORIENTED_EDGE('',*,*,#9989,.F.);
#13956=ORIENTED_EDGE('',*,*,#9771,.F.);
#13957=ORIENTED_EDGE('',*,*,#9989,.T.);
#13958=ORIENTED_EDGE('',*,*,#9543,.T.);
#13959=ORIENTED_EDGE('',*,*,#9985,.F.);
#13960=ORIENTED_EDGE('',*,*,#9772,.F.);
#13961=ORIENTED_EDGE('',*,*,#9980,.T.);
#13962=ORIENTED_EDGE('',*,*,#9547,.T.);
#13963=ORIENTED_EDGE('',*,*,#9990,.F.);
#13964=ORIENTED_EDGE('',*,*,#9768,.F.);
#13965=ORIENTED_EDGE('',*,*,#9990,.T.);
#13966=ORIENTED_EDGE('',*,*,#9546,.T.);
#13967=ORIENTED_EDGE('',*,*,#9981,.F.);
#13968=ORIENTED_EDGE('',*,*,#9769,.F.);
#13969=ORIENTED_EDGE('',*,*,#9978,.T.);
#13970=ORIENTED_EDGE('',*,*,#9550,.T.);
#13971=ORIENTED_EDGE('',*,*,#9991,.F.);
#13972=ORIENTED_EDGE('',*,*,#9765,.F.);
#13973=ORIENTED_EDGE('',*,*,#9991,.T.);
#13974=ORIENTED_EDGE('',*,*,#9549,.T.);
#13975=ORIENTED_EDGE('',*,*,#9979,.F.);
#13976=ORIENTED_EDGE('',*,*,#9766,.F.);
#13977=ORIENTED_EDGE('',*,*,#9976,.T.);
#13978=ORIENTED_EDGE('',*,*,#9553,.T.);
#13979=ORIENTED_EDGE('',*,*,#9992,.F.);
#13980=ORIENTED_EDGE('',*,*,#9762,.F.);
#13981=ORIENTED_EDGE('',*,*,#9992,.T.);
#13982=ORIENTED_EDGE('',*,*,#9552,.T.);
#13983=ORIENTED_EDGE('',*,*,#9977,.F.);
#13984=ORIENTED_EDGE('',*,*,#9763,.F.);
#13985=ORIENTED_EDGE('',*,*,#9974,.T.);
#13986=ORIENTED_EDGE('',*,*,#9556,.T.);
#13987=ORIENTED_EDGE('',*,*,#9993,.F.);
#13988=ORIENTED_EDGE('',*,*,#9759,.F.);
#13989=ORIENTED_EDGE('',*,*,#9993,.T.);
#13990=ORIENTED_EDGE('',*,*,#9555,.T.);
#13991=ORIENTED_EDGE('',*,*,#9975,.F.);
#13992=ORIENTED_EDGE('',*,*,#9760,.F.);
#13993=ORIENTED_EDGE('',*,*,#9972,.T.);
#13994=ORIENTED_EDGE('',*,*,#9559,.T.);
#13995=ORIENTED_EDGE('',*,*,#9994,.F.);
#13996=ORIENTED_EDGE('',*,*,#9756,.F.);
#13997=ORIENTED_EDGE('',*,*,#9994,.T.);
#13998=ORIENTED_EDGE('',*,*,#9558,.T.);
#13999=ORIENTED_EDGE('',*,*,#9973,.F.);
#14000=ORIENTED_EDGE('',*,*,#9757,.F.);
#14001=ORIENTED_EDGE('',*,*,#9970,.T.);
#14002=ORIENTED_EDGE('',*,*,#9562,.T.);
#14003=ORIENTED_EDGE('',*,*,#9995,.F.);
#14004=ORIENTED_EDGE('',*,*,#9753,.F.);
#14005=ORIENTED_EDGE('',*,*,#9995,.T.);
#14006=ORIENTED_EDGE('',*,*,#9561,.T.);
#14007=ORIENTED_EDGE('',*,*,#9971,.F.);
#14008=ORIENTED_EDGE('',*,*,#9754,.F.);
#14009=ORIENTED_EDGE('',*,*,#9968,.T.);
#14010=ORIENTED_EDGE('',*,*,#9565,.T.);
#14011=ORIENTED_EDGE('',*,*,#9996,.F.);
#14012=ORIENTED_EDGE('',*,*,#9750,.F.);
#14013=ORIENTED_EDGE('',*,*,#9996,.T.);
#14014=ORIENTED_EDGE('',*,*,#9564,.T.);
#14015=ORIENTED_EDGE('',*,*,#9969,.F.);
#14016=ORIENTED_EDGE('',*,*,#9751,.F.);
#14017=ORIENTED_EDGE('',*,*,#9966,.T.);
#14018=ORIENTED_EDGE('',*,*,#9568,.T.);
#14019=ORIENTED_EDGE('',*,*,#9997,.F.);
#14020=ORIENTED_EDGE('',*,*,#9747,.F.);
#14021=ORIENTED_EDGE('',*,*,#9997,.T.);
#14022=ORIENTED_EDGE('',*,*,#9567,.T.);
#14023=ORIENTED_EDGE('',*,*,#9967,.F.);
#14024=ORIENTED_EDGE('',*,*,#9748,.F.);
#14025=ORIENTED_EDGE('',*,*,#9964,.T.);
#14026=ORIENTED_EDGE('',*,*,#9571,.T.);
#14027=ORIENTED_EDGE('',*,*,#9998,.F.);
#14028=ORIENTED_EDGE('',*,*,#9744,.F.);
#14029=ORIENTED_EDGE('',*,*,#9998,.T.);
#14030=ORIENTED_EDGE('',*,*,#9570,.T.);
#14031=ORIENTED_EDGE('',*,*,#9965,.F.);
#14032=ORIENTED_EDGE('',*,*,#9745,.F.);
#14033=ORIENTED_EDGE('',*,*,#9962,.T.);
#14034=ORIENTED_EDGE('',*,*,#9574,.T.);
#14035=ORIENTED_EDGE('',*,*,#9999,.F.);
#14036=ORIENTED_EDGE('',*,*,#9741,.F.);
#14037=ORIENTED_EDGE('',*,*,#9999,.T.);
#14038=ORIENTED_EDGE('',*,*,#9573,.T.);
#14039=ORIENTED_EDGE('',*,*,#9963,.F.);
#14040=ORIENTED_EDGE('',*,*,#9742,.F.);
#14041=ORIENTED_EDGE('',*,*,#9960,.T.);
#14042=ORIENTED_EDGE('',*,*,#9577,.T.);
#14043=ORIENTED_EDGE('',*,*,#10000,.F.);
#14044=ORIENTED_EDGE('',*,*,#9738,.F.);
#14045=ORIENTED_EDGE('',*,*,#10000,.T.);
#14046=ORIENTED_EDGE('',*,*,#9576,.T.);
#14047=ORIENTED_EDGE('',*,*,#9961,.F.);
#14048=ORIENTED_EDGE('',*,*,#9739,.F.);
#14049=ORIENTED_EDGE('',*,*,#9958,.T.);
#14050=ORIENTED_EDGE('',*,*,#9580,.T.);
#14051=ORIENTED_EDGE('',*,*,#10001,.F.);
#14052=ORIENTED_EDGE('',*,*,#9735,.F.);
#14053=ORIENTED_EDGE('',*,*,#10001,.T.);
#14054=ORIENTED_EDGE('',*,*,#9579,.T.);
#14055=ORIENTED_EDGE('',*,*,#9959,.F.);
#14056=ORIENTED_EDGE('',*,*,#9736,.F.);
#14057=ORIENTED_EDGE('',*,*,#9956,.T.);
#14058=ORIENTED_EDGE('',*,*,#9583,.T.);
#14059=ORIENTED_EDGE('',*,*,#10002,.F.);
#14060=ORIENTED_EDGE('',*,*,#9732,.F.);
#14061=ORIENTED_EDGE('',*,*,#10002,.T.);
#14062=ORIENTED_EDGE('',*,*,#9582,.T.);
#14063=ORIENTED_EDGE('',*,*,#9957,.F.);
#14064=ORIENTED_EDGE('',*,*,#9733,.F.);
#14065=ORIENTED_EDGE('',*,*,#9954,.T.);
#14066=ORIENTED_EDGE('',*,*,#9586,.T.);
#14067=ORIENTED_EDGE('',*,*,#10003,.F.);
#14068=ORIENTED_EDGE('',*,*,#9729,.F.);
#14069=ORIENTED_EDGE('',*,*,#10003,.T.);
#14070=ORIENTED_EDGE('',*,*,#9585,.T.);
#14071=ORIENTED_EDGE('',*,*,#9955,.F.);
#14072=ORIENTED_EDGE('',*,*,#9730,.F.);
#14073=ORIENTED_EDGE('',*,*,#9952,.T.);
#14074=ORIENTED_EDGE('',*,*,#9589,.T.);
#14075=ORIENTED_EDGE('',*,*,#10004,.F.);
#14076=ORIENTED_EDGE('',*,*,#9726,.F.);
#14077=ORIENTED_EDGE('',*,*,#10004,.T.);
#14078=ORIENTED_EDGE('',*,*,#9588,.T.);
#14079=ORIENTED_EDGE('',*,*,#9953,.F.);
#14080=ORIENTED_EDGE('',*,*,#9727,.F.);
#14081=ORIENTED_EDGE('',*,*,#9950,.T.);
#14082=ORIENTED_EDGE('',*,*,#9592,.T.);
#14083=ORIENTED_EDGE('',*,*,#10005,.F.);
#14084=ORIENTED_EDGE('',*,*,#9723,.F.);
#14085=ORIENTED_EDGE('',*,*,#10005,.T.);
#14086=ORIENTED_EDGE('',*,*,#9591,.T.);
#14087=ORIENTED_EDGE('',*,*,#9951,.F.);
#14088=ORIENTED_EDGE('',*,*,#9724,.F.);
#14089=ORIENTED_EDGE('',*,*,#9948,.T.);
#14090=ORIENTED_EDGE('',*,*,#9595,.T.);
#14091=ORIENTED_EDGE('',*,*,#10006,.F.);
#14092=ORIENTED_EDGE('',*,*,#9720,.F.);
#14093=ORIENTED_EDGE('',*,*,#10006,.T.);
#14094=ORIENTED_EDGE('',*,*,#9594,.T.);
#14095=ORIENTED_EDGE('',*,*,#9949,.F.);
#14096=ORIENTED_EDGE('',*,*,#9721,.F.);
#14097=ORIENTED_EDGE('',*,*,#9946,.T.);
#14098=ORIENTED_EDGE('',*,*,#9364,.T.);
#14099=ORIENTED_EDGE('',*,*,#10007,.F.);
#14100=ORIENTED_EDGE('',*,*,#9717,.F.);
#14101=ORIENTED_EDGE('',*,*,#9714,.F.);
#14102=ORIENTED_EDGE('',*,*,#10007,.T.);
#14103=ORIENTED_EDGE('',*,*,#9597,.T.);
#14104=ORIENTED_EDGE('',*,*,#9947,.F.);
#14105=ORIENTED_EDGE('',*,*,#9718,.F.);
#14106=ORIENTED_EDGE('',*,*,#9944,.T.);
#14107=ORIENTED_EDGE('',*,*,#9367,.T.);
#14108=ORIENTED_EDGE('',*,*,#10008,.F.);
#14109=ORIENTED_EDGE('',*,*,#9711,.F.);
#14110=ORIENTED_EDGE('',*,*,#10008,.T.);
#14111=ORIENTED_EDGE('',*,*,#9366,.T.);
#14112=ORIENTED_EDGE('',*,*,#9945,.F.);
#14113=ORIENTED_EDGE('',*,*,#9712,.F.);
#14114=ORIENTED_EDGE('',*,*,#9942,.T.);
#14115=ORIENTED_EDGE('',*,*,#9370,.T.);
#14116=ORIENTED_EDGE('',*,*,#10009,.F.);
#14117=ORIENTED_EDGE('',*,*,#9708,.F.);
#14118=ORIENTED_EDGE('',*,*,#10009,.T.);
#14119=ORIENTED_EDGE('',*,*,#9369,.T.);
#14120=ORIENTED_EDGE('',*,*,#9943,.F.);
#14121=ORIENTED_EDGE('',*,*,#9709,.F.);
#14122=ORIENTED_EDGE('',*,*,#9940,.T.);
#14123=ORIENTED_EDGE('',*,*,#9373,.T.);
#14124=ORIENTED_EDGE('',*,*,#10010,.F.);
#14125=ORIENTED_EDGE('',*,*,#9705,.F.);
#14126=ORIENTED_EDGE('',*,*,#10010,.T.);
#14127=ORIENTED_EDGE('',*,*,#9372,.T.);
#14128=ORIENTED_EDGE('',*,*,#9941,.F.);
#14129=ORIENTED_EDGE('',*,*,#9706,.F.);
#14130=ORIENTED_EDGE('',*,*,#9938,.T.);
#14131=ORIENTED_EDGE('',*,*,#9376,.T.);
#14132=ORIENTED_EDGE('',*,*,#10011,.F.);
#14133=ORIENTED_EDGE('',*,*,#9702,.F.);
#14134=ORIENTED_EDGE('',*,*,#10011,.T.);
#14135=ORIENTED_EDGE('',*,*,#9375,.T.);
#14136=ORIENTED_EDGE('',*,*,#9939,.F.);
#14137=ORIENTED_EDGE('',*,*,#9703,.F.);
#14138=ORIENTED_EDGE('',*,*,#9936,.T.);
#14139=ORIENTED_EDGE('',*,*,#9379,.T.);
#14140=ORIENTED_EDGE('',*,*,#10012,.F.);
#14141=ORIENTED_EDGE('',*,*,#9699,.F.);
#14142=ORIENTED_EDGE('',*,*,#10012,.T.);
#14143=ORIENTED_EDGE('',*,*,#9378,.T.);
#14144=ORIENTED_EDGE('',*,*,#9937,.F.);
#14145=ORIENTED_EDGE('',*,*,#9700,.F.);
#14146=ORIENTED_EDGE('',*,*,#9934,.T.);
#14147=ORIENTED_EDGE('',*,*,#9382,.T.);
#14148=ORIENTED_EDGE('',*,*,#10013,.F.);
#14149=ORIENTED_EDGE('',*,*,#9696,.F.);
#14150=ORIENTED_EDGE('',*,*,#10013,.T.);
#14151=ORIENTED_EDGE('',*,*,#9381,.T.);
#14152=ORIENTED_EDGE('',*,*,#9935,.F.);
#14153=ORIENTED_EDGE('',*,*,#9697,.F.);
#14154=ORIENTED_EDGE('',*,*,#9932,.T.);
#14155=ORIENTED_EDGE('',*,*,#9385,.T.);
#14156=ORIENTED_EDGE('',*,*,#10014,.F.);
#14157=ORIENTED_EDGE('',*,*,#9693,.F.);
#14158=ORIENTED_EDGE('',*,*,#10014,.T.);
#14159=ORIENTED_EDGE('',*,*,#9384,.T.);
#14160=ORIENTED_EDGE('',*,*,#9933,.F.);
#14161=ORIENTED_EDGE('',*,*,#9694,.F.);
#14162=ORIENTED_EDGE('',*,*,#9930,.T.);
#14163=ORIENTED_EDGE('',*,*,#9388,.T.);
#14164=ORIENTED_EDGE('',*,*,#10015,.F.);
#14165=ORIENTED_EDGE('',*,*,#9690,.F.);
#14166=ORIENTED_EDGE('',*,*,#10015,.T.);
#14167=ORIENTED_EDGE('',*,*,#9387,.T.);
#14168=ORIENTED_EDGE('',*,*,#9931,.F.);
#14169=ORIENTED_EDGE('',*,*,#9691,.F.);
#14170=ORIENTED_EDGE('',*,*,#9928,.T.);
#14171=ORIENTED_EDGE('',*,*,#9391,.T.);
#14172=ORIENTED_EDGE('',*,*,#10016,.F.);
#14173=ORIENTED_EDGE('',*,*,#9687,.F.);
#14174=ORIENTED_EDGE('',*,*,#10016,.T.);
#14175=ORIENTED_EDGE('',*,*,#9390,.T.);
#14176=ORIENTED_EDGE('',*,*,#9929,.F.);
#14177=ORIENTED_EDGE('',*,*,#9688,.F.);
#14178=ORIENTED_EDGE('',*,*,#9926,.T.);
#14179=ORIENTED_EDGE('',*,*,#9394,.T.);
#14180=ORIENTED_EDGE('',*,*,#10017,.F.);
#14181=ORIENTED_EDGE('',*,*,#9684,.F.);
#14182=ORIENTED_EDGE('',*,*,#10017,.T.);
#14183=ORIENTED_EDGE('',*,*,#9393,.T.);
#14184=ORIENTED_EDGE('',*,*,#9927,.F.);
#14185=ORIENTED_EDGE('',*,*,#9685,.F.);
#14186=ORIENTED_EDGE('',*,*,#9924,.T.);
#14187=ORIENTED_EDGE('',*,*,#9397,.T.);
#14188=ORIENTED_EDGE('',*,*,#10018,.F.);
#14189=ORIENTED_EDGE('',*,*,#9681,.F.);
#14190=ORIENTED_EDGE('',*,*,#10018,.T.);
#14191=ORIENTED_EDGE('',*,*,#9396,.T.);
#14192=ORIENTED_EDGE('',*,*,#9925,.F.);
#14193=ORIENTED_EDGE('',*,*,#9682,.F.);
#14194=ORIENTED_EDGE('',*,*,#9922,.T.);
#14195=ORIENTED_EDGE('',*,*,#9400,.T.);
#14196=ORIENTED_EDGE('',*,*,#10019,.F.);
#14197=ORIENTED_EDGE('',*,*,#9678,.F.);
#14198=ORIENTED_EDGE('',*,*,#10019,.T.);
#14199=ORIENTED_EDGE('',*,*,#9399,.T.);
#14200=ORIENTED_EDGE('',*,*,#9923,.F.);
#14201=ORIENTED_EDGE('',*,*,#9679,.F.);
#14202=ORIENTED_EDGE('',*,*,#9920,.T.);
#14203=ORIENTED_EDGE('',*,*,#9403,.T.);
#14204=ORIENTED_EDGE('',*,*,#10020,.F.);
#14205=ORIENTED_EDGE('',*,*,#9675,.F.);
#14206=ORIENTED_EDGE('',*,*,#10020,.T.);
#14207=ORIENTED_EDGE('',*,*,#9402,.T.);
#14208=ORIENTED_EDGE('',*,*,#9921,.F.);
#14209=ORIENTED_EDGE('',*,*,#9676,.F.);
#14210=ORIENTED_EDGE('',*,*,#9918,.T.);
#14211=ORIENTED_EDGE('',*,*,#9406,.T.);
#14212=ORIENTED_EDGE('',*,*,#10021,.F.);
#14213=ORIENTED_EDGE('',*,*,#9672,.F.);
#14214=ORIENTED_EDGE('',*,*,#10021,.T.);
#14215=ORIENTED_EDGE('',*,*,#9405,.T.);
#14216=ORIENTED_EDGE('',*,*,#9919,.F.);
#14217=ORIENTED_EDGE('',*,*,#9673,.F.);
#14218=ORIENTED_EDGE('',*,*,#9916,.T.);
#14219=ORIENTED_EDGE('',*,*,#9409,.T.);
#14220=ORIENTED_EDGE('',*,*,#10022,.F.);
#14221=ORIENTED_EDGE('',*,*,#9669,.F.);
#14222=ORIENTED_EDGE('',*,*,#10022,.T.);
#14223=ORIENTED_EDGE('',*,*,#9408,.T.);
#14224=ORIENTED_EDGE('',*,*,#9917,.F.);
#14225=ORIENTED_EDGE('',*,*,#9670,.F.);
#14226=ORIENTED_EDGE('',*,*,#9914,.T.);
#14227=ORIENTED_EDGE('',*,*,#9412,.T.);
#14228=ORIENTED_EDGE('',*,*,#10023,.F.);
#14229=ORIENTED_EDGE('',*,*,#9666,.F.);
#14230=ORIENTED_EDGE('',*,*,#10023,.T.);
#14231=ORIENTED_EDGE('',*,*,#9411,.T.);
#14232=ORIENTED_EDGE('',*,*,#9915,.F.);
#14233=ORIENTED_EDGE('',*,*,#9667,.F.);
#14234=ORIENTED_EDGE('',*,*,#9912,.T.);
#14235=ORIENTED_EDGE('',*,*,#9415,.T.);
#14236=ORIENTED_EDGE('',*,*,#10024,.F.);
#14237=ORIENTED_EDGE('',*,*,#9663,.F.);
#14238=ORIENTED_EDGE('',*,*,#10024,.T.);
#14239=ORIENTED_EDGE('',*,*,#9414,.T.);
#14240=ORIENTED_EDGE('',*,*,#9913,.F.);
#14241=ORIENTED_EDGE('',*,*,#9664,.F.);
#14242=ORIENTED_EDGE('',*,*,#9910,.T.);
#14243=ORIENTED_EDGE('',*,*,#9418,.T.);
#14244=ORIENTED_EDGE('',*,*,#10025,.F.);
#14245=ORIENTED_EDGE('',*,*,#9660,.F.);
#14246=ORIENTED_EDGE('',*,*,#10025,.T.);
#14247=ORIENTED_EDGE('',*,*,#9417,.T.);
#14248=ORIENTED_EDGE('',*,*,#9911,.F.);
#14249=ORIENTED_EDGE('',*,*,#9661,.F.);
#14250=ORIENTED_EDGE('',*,*,#9908,.T.);
#14251=ORIENTED_EDGE('',*,*,#9421,.T.);
#14252=ORIENTED_EDGE('',*,*,#10026,.F.);
#14253=ORIENTED_EDGE('',*,*,#9657,.F.);
#14254=ORIENTED_EDGE('',*,*,#10026,.T.);
#14255=ORIENTED_EDGE('',*,*,#9420,.T.);
#14256=ORIENTED_EDGE('',*,*,#9909,.F.);
#14257=ORIENTED_EDGE('',*,*,#9658,.F.);
#14258=ORIENTED_EDGE('',*,*,#9906,.T.);
#14259=ORIENTED_EDGE('',*,*,#9424,.T.);
#14260=ORIENTED_EDGE('',*,*,#10027,.F.);
#14261=ORIENTED_EDGE('',*,*,#9654,.F.);
#14262=ORIENTED_EDGE('',*,*,#10027,.T.);
#14263=ORIENTED_EDGE('',*,*,#9423,.T.);
#14264=ORIENTED_EDGE('',*,*,#9907,.F.);
#14265=ORIENTED_EDGE('',*,*,#9655,.F.);
#14266=ORIENTED_EDGE('',*,*,#9904,.T.);
#14267=ORIENTED_EDGE('',*,*,#9427,.T.);
#14268=ORIENTED_EDGE('',*,*,#10028,.F.);
#14269=ORIENTED_EDGE('',*,*,#9651,.F.);
#14270=ORIENTED_EDGE('',*,*,#10028,.T.);
#14271=ORIENTED_EDGE('',*,*,#9426,.T.);
#14272=ORIENTED_EDGE('',*,*,#9905,.F.);
#14273=ORIENTED_EDGE('',*,*,#9652,.F.);
#14274=ORIENTED_EDGE('',*,*,#9902,.T.);
#14275=ORIENTED_EDGE('',*,*,#9430,.T.);
#14276=ORIENTED_EDGE('',*,*,#10029,.F.);
#14277=ORIENTED_EDGE('',*,*,#9648,.F.);
#14278=ORIENTED_EDGE('',*,*,#10029,.T.);
#14279=ORIENTED_EDGE('',*,*,#9429,.T.);
#14280=ORIENTED_EDGE('',*,*,#9903,.F.);
#14281=ORIENTED_EDGE('',*,*,#9649,.F.);
#14282=ORIENTED_EDGE('',*,*,#9900,.T.);
#14283=ORIENTED_EDGE('',*,*,#9433,.T.);
#14284=ORIENTED_EDGE('',*,*,#10030,.F.);
#14285=ORIENTED_EDGE('',*,*,#9645,.F.);
#14286=ORIENTED_EDGE('',*,*,#10030,.T.);
#14287=ORIENTED_EDGE('',*,*,#9432,.T.);
#14288=ORIENTED_EDGE('',*,*,#9901,.F.);
#14289=ORIENTED_EDGE('',*,*,#9646,.F.);
#14290=ORIENTED_EDGE('',*,*,#9898,.T.);
#14291=ORIENTED_EDGE('',*,*,#9436,.T.);
#14292=ORIENTED_EDGE('',*,*,#10031,.F.);
#14293=ORIENTED_EDGE('',*,*,#9642,.F.);
#14294=ORIENTED_EDGE('',*,*,#10031,.T.);
#14295=ORIENTED_EDGE('',*,*,#9435,.T.);
#14296=ORIENTED_EDGE('',*,*,#9899,.F.);
#14297=ORIENTED_EDGE('',*,*,#9643,.F.);
#14298=ORIENTED_EDGE('',*,*,#9896,.T.);
#14299=ORIENTED_EDGE('',*,*,#9439,.T.);
#14300=ORIENTED_EDGE('',*,*,#10032,.F.);
#14301=ORIENTED_EDGE('',*,*,#9639,.F.);
#14302=ORIENTED_EDGE('',*,*,#10032,.T.);
#14303=ORIENTED_EDGE('',*,*,#9438,.T.);
#14304=ORIENTED_EDGE('',*,*,#9897,.F.);
#14305=ORIENTED_EDGE('',*,*,#9640,.F.);
#14306=ORIENTED_EDGE('',*,*,#9894,.T.);
#14307=ORIENTED_EDGE('',*,*,#9442,.T.);
#14308=ORIENTED_EDGE('',*,*,#10033,.F.);
#14309=ORIENTED_EDGE('',*,*,#9636,.F.);
#14310=ORIENTED_EDGE('',*,*,#10033,.T.);
#14311=ORIENTED_EDGE('',*,*,#9441,.T.);
#14312=ORIENTED_EDGE('',*,*,#9895,.F.);
#14313=ORIENTED_EDGE('',*,*,#9637,.F.);
#14314=ORIENTED_EDGE('',*,*,#9892,.T.);
#14315=ORIENTED_EDGE('',*,*,#9445,.T.);
#14316=ORIENTED_EDGE('',*,*,#10034,.F.);
#14317=ORIENTED_EDGE('',*,*,#9633,.F.);
#14318=ORIENTED_EDGE('',*,*,#10034,.T.);
#14319=ORIENTED_EDGE('',*,*,#9444,.T.);
#14320=ORIENTED_EDGE('',*,*,#9893,.F.);
#14321=ORIENTED_EDGE('',*,*,#9634,.F.);
#14322=ORIENTED_EDGE('',*,*,#9890,.T.);
#14323=ORIENTED_EDGE('',*,*,#9448,.T.);
#14324=ORIENTED_EDGE('',*,*,#10035,.F.);
#14325=ORIENTED_EDGE('',*,*,#9630,.F.);
#14326=ORIENTED_EDGE('',*,*,#10035,.T.);
#14327=ORIENTED_EDGE('',*,*,#9447,.T.);
#14328=ORIENTED_EDGE('',*,*,#9891,.F.);
#14329=ORIENTED_EDGE('',*,*,#9631,.F.);
#14330=ORIENTED_EDGE('',*,*,#9888,.T.);
#14331=ORIENTED_EDGE('',*,*,#9451,.T.);
#14332=ORIENTED_EDGE('',*,*,#10036,.F.);
#14333=ORIENTED_EDGE('',*,*,#9627,.F.);
#14334=ORIENTED_EDGE('',*,*,#10036,.T.);
#14335=ORIENTED_EDGE('',*,*,#9450,.T.);
#14336=ORIENTED_EDGE('',*,*,#9889,.F.);
#14337=ORIENTED_EDGE('',*,*,#9628,.F.);
#14338=ORIENTED_EDGE('',*,*,#9886,.T.);
#14339=ORIENTED_EDGE('',*,*,#9454,.T.);
#14340=ORIENTED_EDGE('',*,*,#10037,.F.);
#14341=ORIENTED_EDGE('',*,*,#9624,.F.);
#14342=ORIENTED_EDGE('',*,*,#10037,.T.);
#14343=ORIENTED_EDGE('',*,*,#9453,.T.);
#14344=ORIENTED_EDGE('',*,*,#9887,.F.);
#14345=ORIENTED_EDGE('',*,*,#9625,.F.);
#14346=ORIENTED_EDGE('',*,*,#9884,.T.);
#14347=ORIENTED_EDGE('',*,*,#9457,.T.);
#14348=ORIENTED_EDGE('',*,*,#10038,.F.);
#14349=ORIENTED_EDGE('',*,*,#9621,.F.);
#14350=ORIENTED_EDGE('',*,*,#10038,.T.);
#14351=ORIENTED_EDGE('',*,*,#9456,.T.);
#14352=ORIENTED_EDGE('',*,*,#9885,.F.);
#14353=ORIENTED_EDGE('',*,*,#9622,.F.);
#14354=ORIENTED_EDGE('',*,*,#9882,.T.);
#14355=ORIENTED_EDGE('',*,*,#9460,.T.);
#14356=ORIENTED_EDGE('',*,*,#10039,.F.);
#14357=ORIENTED_EDGE('',*,*,#9618,.F.);
#14358=ORIENTED_EDGE('',*,*,#10039,.T.);
#14359=ORIENTED_EDGE('',*,*,#9459,.T.);
#14360=ORIENTED_EDGE('',*,*,#9883,.F.);
#14361=ORIENTED_EDGE('',*,*,#9619,.F.);
#14362=ORIENTED_EDGE('',*,*,#9880,.T.);
#14363=ORIENTED_EDGE('',*,*,#9463,.T.);
#14364=ORIENTED_EDGE('',*,*,#10040,.F.);
#14365=ORIENTED_EDGE('',*,*,#9615,.F.);
#14366=ORIENTED_EDGE('',*,*,#10040,.T.);
#14367=ORIENTED_EDGE('',*,*,#9462,.T.);
#14368=ORIENTED_EDGE('',*,*,#9881,.F.);
#14369=ORIENTED_EDGE('',*,*,#9616,.F.);
#14370=ORIENTED_EDGE('',*,*,#9878,.T.);
#14371=ORIENTED_EDGE('',*,*,#9466,.T.);
#14372=ORIENTED_EDGE('',*,*,#10041,.F.);
#14373=ORIENTED_EDGE('',*,*,#9612,.F.);
#14374=ORIENTED_EDGE('',*,*,#10041,.T.);
#14375=ORIENTED_EDGE('',*,*,#9465,.T.);
#14376=ORIENTED_EDGE('',*,*,#9879,.F.);
#14377=ORIENTED_EDGE('',*,*,#9613,.F.);
#14378=ORIENTED_EDGE('',*,*,#9876,.T.);
#14379=ORIENTED_EDGE('',*,*,#9469,.T.);
#14380=ORIENTED_EDGE('',*,*,#10042,.F.);
#14381=ORIENTED_EDGE('',*,*,#9609,.F.);
#14382=ORIENTED_EDGE('',*,*,#10042,.T.);
#14383=ORIENTED_EDGE('',*,*,#9468,.T.);
#14384=ORIENTED_EDGE('',*,*,#9877,.F.);
#14385=ORIENTED_EDGE('',*,*,#9610,.F.);
#14386=ORIENTED_EDGE('',*,*,#9874,.T.);
#14387=ORIENTED_EDGE('',*,*,#9472,.T.);
#14388=ORIENTED_EDGE('',*,*,#10043,.F.);
#14389=ORIENTED_EDGE('',*,*,#9606,.F.);
#14390=ORIENTED_EDGE('',*,*,#10043,.T.);
#14391=ORIENTED_EDGE('',*,*,#9471,.T.);
#14392=ORIENTED_EDGE('',*,*,#9875,.F.);
#14393=ORIENTED_EDGE('',*,*,#9607,.F.);
#14394=ORIENTED_EDGE('',*,*,#9872,.T.);
#14395=ORIENTED_EDGE('',*,*,#9475,.T.);
#14396=ORIENTED_EDGE('',*,*,#10044,.F.);
#14397=ORIENTED_EDGE('',*,*,#9603,.F.);
#14398=ORIENTED_EDGE('',*,*,#10044,.T.);
#14399=ORIENTED_EDGE('',*,*,#9474,.T.);
#14400=ORIENTED_EDGE('',*,*,#9873,.F.);
#14401=ORIENTED_EDGE('',*,*,#9604,.F.);
#14402=ORIENTED_EDGE('',*,*,#9870,.T.);
#14403=ORIENTED_EDGE('',*,*,#9478,.T.);
#14404=ORIENTED_EDGE('',*,*,#10045,.F.);
#14405=ORIENTED_EDGE('',*,*,#9600,.F.);
#14406=ORIENTED_EDGE('',*,*,#10045,.T.);
#14407=ORIENTED_EDGE('',*,*,#9477,.T.);
#14408=ORIENTED_EDGE('',*,*,#9871,.F.);
#14409=ORIENTED_EDGE('',*,*,#9601,.F.);
#14410=ORIENTED_EDGE('',*,*,#9868,.T.);
#14411=ORIENTED_EDGE('',*,*,#9484,.T.);
#14412=ORIENTED_EDGE('',*,*,#10046,.F.);
#14413=ORIENTED_EDGE('',*,*,#9831,.F.);
#14414=ORIENTED_EDGE('',*,*,#10046,.T.);
#14415=ORIENTED_EDGE('',*,*,#9483,.T.);
#14416=ORIENTED_EDGE('',*,*,#9480,.T.);
#14417=ORIENTED_EDGE('',*,*,#9869,.F.);
#14418=ORIENTED_EDGE('',*,*,#9598,.F.);
#14419=ORIENTED_EDGE('',*,*,#9866,.T.);
#14420=ORIENTED_EDGE('',*,*,#9487,.T.);
#14421=ORIENTED_EDGE('',*,*,#10047,.F.);
#14422=ORIENTED_EDGE('',*,*,#9828,.F.);
#14423=ORIENTED_EDGE('',*,*,#10047,.T.);
#14424=ORIENTED_EDGE('',*,*,#9486,.T.);
#14425=ORIENTED_EDGE('',*,*,#9867,.F.);
#14426=ORIENTED_EDGE('',*,*,#9829,.F.);
#14427=ORIENTED_EDGE('',*,*,#9864,.T.);
#14428=ORIENTED_EDGE('',*,*,#9490,.T.);
#14429=ORIENTED_EDGE('',*,*,#10048,.F.);
#14430=ORIENTED_EDGE('',*,*,#9825,.F.);
#14431=ORIENTED_EDGE('',*,*,#10048,.T.);
#14432=ORIENTED_EDGE('',*,*,#9489,.T.);
#14433=ORIENTED_EDGE('',*,*,#9865,.F.);
#14434=ORIENTED_EDGE('',*,*,#9826,.F.);
#14435=ORIENTED_EDGE('',*,*,#9862,.T.);
#14436=ORIENTED_EDGE('',*,*,#9493,.T.);
#14437=ORIENTED_EDGE('',*,*,#10049,.F.);
#14438=ORIENTED_EDGE('',*,*,#9822,.F.);
#14439=ORIENTED_EDGE('',*,*,#10049,.T.);
#14440=ORIENTED_EDGE('',*,*,#9492,.T.);
#14441=ORIENTED_EDGE('',*,*,#9863,.F.);
#14442=ORIENTED_EDGE('',*,*,#9823,.F.);
#14443=ORIENTED_EDGE('',*,*,#9860,.T.);
#14444=ORIENTED_EDGE('',*,*,#9496,.T.);
#14445=ORIENTED_EDGE('',*,*,#10050,.F.);
#14446=ORIENTED_EDGE('',*,*,#9819,.F.);
#14447=ORIENTED_EDGE('',*,*,#10050,.T.);
#14448=ORIENTED_EDGE('',*,*,#9495,.T.);
#14449=ORIENTED_EDGE('',*,*,#9861,.F.);
#14450=ORIENTED_EDGE('',*,*,#9820,.F.);
#14451=ORIENTED_EDGE('',*,*,#9858,.T.);
#14452=ORIENTED_EDGE('',*,*,#9499,.T.);
#14453=ORIENTED_EDGE('',*,*,#10051,.F.);
#14454=ORIENTED_EDGE('',*,*,#9816,.F.);
#14455=ORIENTED_EDGE('',*,*,#10051,.T.);
#14456=ORIENTED_EDGE('',*,*,#9498,.T.);
#14457=ORIENTED_EDGE('',*,*,#9859,.F.);
#14458=ORIENTED_EDGE('',*,*,#9817,.F.);
#14459=ORIENTED_EDGE('',*,*,#9856,.T.);
#14460=ORIENTED_EDGE('',*,*,#9502,.T.);
#14461=ORIENTED_EDGE('',*,*,#10052,.F.);
#14462=ORIENTED_EDGE('',*,*,#9813,.F.);
#14463=ORIENTED_EDGE('',*,*,#10052,.T.);
#14464=ORIENTED_EDGE('',*,*,#9501,.T.);
#14465=ORIENTED_EDGE('',*,*,#9857,.F.);
#14466=ORIENTED_EDGE('',*,*,#9814,.F.);
#14467=ORIENTED_EDGE('',*,*,#9854,.T.);
#14468=ORIENTED_EDGE('',*,*,#9505,.T.);
#14469=ORIENTED_EDGE('',*,*,#10053,.F.);
#14470=ORIENTED_EDGE('',*,*,#9810,.F.);
#14471=ORIENTED_EDGE('',*,*,#10053,.T.);
#14472=ORIENTED_EDGE('',*,*,#9504,.T.);
#14473=ORIENTED_EDGE('',*,*,#9855,.F.);
#14474=ORIENTED_EDGE('',*,*,#9811,.F.);
#14475=ORIENTED_EDGE('',*,*,#9852,.T.);
#14476=ORIENTED_EDGE('',*,*,#9508,.T.);
#14477=ORIENTED_EDGE('',*,*,#10054,.F.);
#14478=ORIENTED_EDGE('',*,*,#9807,.F.);
#14479=ORIENTED_EDGE('',*,*,#10054,.T.);
#14480=ORIENTED_EDGE('',*,*,#9507,.T.);
#14481=ORIENTED_EDGE('',*,*,#9853,.F.);
#14482=ORIENTED_EDGE('',*,*,#9808,.F.);
#14483=ORIENTED_EDGE('',*,*,#9850,.T.);
#14484=ORIENTED_EDGE('',*,*,#9511,.T.);
#14485=ORIENTED_EDGE('',*,*,#10055,.F.);
#14486=ORIENTED_EDGE('',*,*,#9804,.F.);
#14487=ORIENTED_EDGE('',*,*,#10055,.T.);
#14488=ORIENTED_EDGE('',*,*,#9510,.T.);
#14489=ORIENTED_EDGE('',*,*,#9851,.F.);
#14490=ORIENTED_EDGE('',*,*,#9805,.F.);
#14491=ORIENTED_EDGE('',*,*,#9848,.T.);
#14492=ORIENTED_EDGE('',*,*,#9514,.T.);
#14493=ORIENTED_EDGE('',*,*,#10056,.F.);
#14494=ORIENTED_EDGE('',*,*,#9801,.F.);
#14495=ORIENTED_EDGE('',*,*,#10056,.T.);
#14496=ORIENTED_EDGE('',*,*,#9513,.T.);
#14497=ORIENTED_EDGE('',*,*,#9849,.F.);
#14498=ORIENTED_EDGE('',*,*,#9802,.F.);
#14499=ORIENTED_EDGE('',*,*,#9846,.T.);
#14500=ORIENTED_EDGE('',*,*,#9517,.T.);
#14501=ORIENTED_EDGE('',*,*,#10057,.F.);
#14502=ORIENTED_EDGE('',*,*,#9798,.F.);
#14503=ORIENTED_EDGE('',*,*,#10057,.T.);
#14504=ORIENTED_EDGE('',*,*,#9516,.T.);
#14505=ORIENTED_EDGE('',*,*,#9847,.F.);
#14506=ORIENTED_EDGE('',*,*,#9799,.F.);
#14507=ORIENTED_EDGE('',*,*,#9844,.T.);
#14508=ORIENTED_EDGE('',*,*,#9520,.T.);
#14509=ORIENTED_EDGE('',*,*,#10058,.F.);
#14510=ORIENTED_EDGE('',*,*,#9795,.F.);
#14511=ORIENTED_EDGE('',*,*,#10058,.T.);
#14512=ORIENTED_EDGE('',*,*,#9519,.T.);
#14513=ORIENTED_EDGE('',*,*,#9845,.F.);
#14514=ORIENTED_EDGE('',*,*,#9796,.F.);
#14515=ORIENTED_EDGE('',*,*,#9842,.T.);
#14516=ORIENTED_EDGE('',*,*,#9523,.T.);
#14517=ORIENTED_EDGE('',*,*,#10059,.F.);
#14518=ORIENTED_EDGE('',*,*,#9792,.F.);
#14519=ORIENTED_EDGE('',*,*,#10059,.T.);
#14520=ORIENTED_EDGE('',*,*,#9522,.T.);
#14521=ORIENTED_EDGE('',*,*,#9843,.F.);
#14522=ORIENTED_EDGE('',*,*,#9793,.F.);
#14523=ORIENTED_EDGE('',*,*,#9840,.T.);
#14524=ORIENTED_EDGE('',*,*,#9526,.T.);
#14525=ORIENTED_EDGE('',*,*,#10060,.F.);
#14526=ORIENTED_EDGE('',*,*,#9789,.F.);
#14527=ORIENTED_EDGE('',*,*,#10060,.T.);
#14528=ORIENTED_EDGE('',*,*,#9525,.T.);
#14529=ORIENTED_EDGE('',*,*,#9841,.F.);
#14530=ORIENTED_EDGE('',*,*,#9790,.F.);
#14531=ORIENTED_EDGE('',*,*,#9838,.T.);
#14532=ORIENTED_EDGE('',*,*,#9529,.T.);
#14533=ORIENTED_EDGE('',*,*,#10061,.F.);
#14534=ORIENTED_EDGE('',*,*,#9786,.F.);
#14535=ORIENTED_EDGE('',*,*,#10061,.T.);
#14536=ORIENTED_EDGE('',*,*,#9528,.T.);
#14537=ORIENTED_EDGE('',*,*,#9839,.F.);
#14538=ORIENTED_EDGE('',*,*,#9787,.F.);
#14539=ORIENTED_EDGE('',*,*,#9836,.T.);
#14540=ORIENTED_EDGE('',*,*,#9532,.T.);
#14541=ORIENTED_EDGE('',*,*,#10062,.F.);
#14542=ORIENTED_EDGE('',*,*,#9783,.F.);
#14543=ORIENTED_EDGE('',*,*,#10062,.T.);
#14544=ORIENTED_EDGE('',*,*,#9531,.T.);
#14545=ORIENTED_EDGE('',*,*,#9837,.F.);
#14546=ORIENTED_EDGE('',*,*,#9784,.F.);
#14547=ORIENTED_EDGE('',*,*,#9833,.T.);
#14548=ORIENTED_EDGE('',*,*,#9535,.T.);
#14549=ORIENTED_EDGE('',*,*,#10063,.F.);
#14550=ORIENTED_EDGE('',*,*,#9780,.F.);
#14551=ORIENTED_EDGE('',*,*,#10063,.T.);
#14552=ORIENTED_EDGE('',*,*,#9534,.T.);
#14553=ORIENTED_EDGE('',*,*,#9835,.F.);
#14554=ORIENTED_EDGE('',*,*,#9781,.F.);
#14555=ORIENTED_EDGE('',*,*,#10064,.T.);
#14556=ORIENTED_EDGE('',*,*,#10065,.F.);
#14557=ORIENTED_EDGE('',*,*,#10066,.F.);
#14558=ORIENTED_EDGE('',*,*,#10067,.F.);
#14559=ORIENTED_EDGE('',*,*,#10068,.T.);
#14560=ORIENTED_EDGE('',*,*,#10069,.T.);
#14561=ORIENTED_EDGE('',*,*,#10070,.F.);
#14562=ORIENTED_EDGE('',*,*,#10071,.F.);
#14563=ORIENTED_EDGE('',*,*,#10069,.F.);
#14564=ORIENTED_EDGE('',*,*,#10072,.T.);
#14565=ORIENTED_EDGE('',*,*,#10073,.F.);
#14566=ORIENTED_EDGE('',*,*,#10074,.F.);
#14567=ORIENTED_EDGE('',*,*,#10075,.F.);
#14568=ORIENTED_EDGE('',*,*,#10076,.T.);
#14569=ORIENTED_EDGE('',*,*,#10077,.T.);
#14570=ORIENTED_EDGE('',*,*,#10070,.T.);
#14571=ORIENTED_EDGE('',*,*,#10071,.T.);
#14572=ORIENTED_EDGE('',*,*,#10077,.F.);
#14573=ORIENTED_EDGE('',*,*,#10078,.F.);
#14574=ORIENTED_EDGE('',*,*,#10079,.T.);
#14575=ORIENTED_EDGE('',*,*,#10080,.T.);
#14576=ORIENTED_EDGE('',*,*,#10079,.F.);
#14577=ORIENTED_EDGE('',*,*,#10081,.F.);
#14578=ORIENTED_EDGE('',*,*,#10074,.T.);
#14579=ORIENTED_EDGE('',*,*,#10080,.F.);
#14580=ORIENTED_EDGE('',*,*,#10082,.F.);
#14581=ORIENTED_EDGE('',*,*,#10066,.T.);
#14582=ORIENTED_EDGE('',*,*,#10076,.F.);
#14583=ORIENTED_EDGE('',*,*,#10078,.T.);
#14584=ORIENTED_EDGE('',*,*,#10073,.T.);
#14585=ORIENTED_EDGE('',*,*,#10083,.F.);
#14586=ORIENTED_EDGE('',*,*,#10075,.T.);
#14587=ORIENTED_EDGE('',*,*,#10081,.T.);
#14588=ORIENTED_EDGE('',*,*,#10067,.T.);
#14589=ORIENTED_EDGE('',*,*,#10082,.T.);
#14590=ORIENTED_EDGE('',*,*,#10065,.T.);
#14591=ORIENTED_EDGE('',*,*,#10084,.F.);
#14592=ORIENTED_EDGE('',*,*,#10084,.T.);
#14593=ORIENTED_EDGE('',*,*,#10064,.F.);
#14594=ORIENTED_EDGE('',*,*,#10083,.T.);
#14595=ORIENTED_EDGE('',*,*,#10072,.F.);
#14596=ORIENTED_EDGE('',*,*,#10068,.F.);
#14597=ORIENTED_EDGE('',*,*,#10085,.F.);
#14598=ORIENTED_EDGE('',*,*,#10086,.T.);
#14599=ORIENTED_EDGE('',*,*,#10087,.F.);
#14600=ORIENTED_EDGE('',*,*,#10086,.F.);
#14601=ORIENTED_EDGE('',*,*,#10088,.F.);
#14602=ORIENTED_EDGE('',*,*,#10089,.F.);
#14603=ORIENTED_EDGE('',*,*,#10090,.T.);
#14604=ORIENTED_EDGE('',*,*,#10091,.T.);
#14605=ORIENTED_EDGE('',*,*,#10090,.F.);
#14606=ORIENTED_EDGE('',*,*,#10092,.F.);
#14607=ORIENTED_EDGE('',*,*,#10093,.F.);
#14608=ORIENTED_EDGE('',*,*,#10094,.T.);
#14609=ORIENTED_EDGE('',*,*,#10095,.T.);
#14610=ORIENTED_EDGE('',*,*,#10096,.T.);
#14611=ORIENTED_EDGE('',*,*,#10094,.F.);
#14612=ORIENTED_EDGE('',*,*,#10088,.T.);
#14613=ORIENTED_EDGE('',*,*,#10089,.T.);
#14614=ORIENTED_EDGE('',*,*,#10097,.T.);
#14615=ORIENTED_EDGE('',*,*,#10095,.F.);
#14616=ORIENTED_EDGE('',*,*,#10096,.F.);
#14617=ORIENTED_EDGE('',*,*,#10097,.F.);
#14618=ORIENTED_EDGE('',*,*,#10098,.F.);
#14619=ORIENTED_EDGE('',*,*,#10099,.F.);
#14620=ORIENTED_EDGE('',*,*,#10100,.T.);
#14621=ORIENTED_EDGE('',*,*,#10092,.T.);
#14622=ORIENTED_EDGE('',*,*,#10093,.T.);
#14623=ORIENTED_EDGE('',*,*,#10100,.F.);
#14624=ORIENTED_EDGE('',*,*,#10101,.F.);
#14625=ORIENTED_EDGE('',*,*,#10102,.F.);
#14626=ORIENTED_EDGE('',*,*,#10103,.T.);
#14627=ORIENTED_EDGE('',*,*,#10104,.T.);
#14628=ORIENTED_EDGE('',*,*,#10105,.T.);
#14629=ORIENTED_EDGE('',*,*,#10103,.F.);
#14630=ORIENTED_EDGE('',*,*,#10098,.T.);
#14631=ORIENTED_EDGE('',*,*,#10099,.T.);
#14632=ORIENTED_EDGE('',*,*,#10106,.T.);
#14633=ORIENTED_EDGE('',*,*,#10104,.F.);
#14634=ORIENTED_EDGE('',*,*,#10105,.F.);
#14635=ORIENTED_EDGE('',*,*,#10106,.F.);
#14636=ORIENTED_EDGE('',*,*,#10107,.F.);
#14637=ORIENTED_EDGE('',*,*,#10108,.F.);
#14638=ORIENTED_EDGE('',*,*,#10109,.T.);
#14639=ORIENTED_EDGE('',*,*,#10101,.T.);
#14640=ORIENTED_EDGE('',*,*,#10102,.T.);
#14641=ORIENTED_EDGE('',*,*,#10109,.F.);
#14642=ORIENTED_EDGE('',*,*,#10110,.F.);
#14643=ORIENTED_EDGE('',*,*,#10111,.F.);
#14644=ORIENTED_EDGE('',*,*,#10112,.T.);
#14645=ORIENTED_EDGE('',*,*,#10113,.T.);
#14646=ORIENTED_EDGE('',*,*,#10114,.T.);
#14647=ORIENTED_EDGE('',*,*,#10112,.F.);
#14648=ORIENTED_EDGE('',*,*,#10107,.T.);
#14649=ORIENTED_EDGE('',*,*,#10108,.T.);
#14650=ORIENTED_EDGE('',*,*,#10115,.T.);
#14651=ORIENTED_EDGE('',*,*,#10113,.F.);
#14652=ORIENTED_EDGE('',*,*,#10114,.F.);
#14653=ORIENTED_EDGE('',*,*,#10115,.F.);
#14654=ORIENTED_EDGE('',*,*,#10116,.F.);
#14655=ORIENTED_EDGE('',*,*,#10117,.F.);
#14656=ORIENTED_EDGE('',*,*,#10118,.T.);
#14657=ORIENTED_EDGE('',*,*,#10110,.T.);
#14658=ORIENTED_EDGE('',*,*,#10111,.T.);
#14659=ORIENTED_EDGE('',*,*,#10118,.F.);
#14660=ORIENTED_EDGE('',*,*,#10119,.F.);
#14661=ORIENTED_EDGE('',*,*,#10120,.F.);
#14662=ORIENTED_EDGE('',*,*,#10121,.T.);
#14663=ORIENTED_EDGE('',*,*,#10122,.T.);
#14664=ORIENTED_EDGE('',*,*,#10123,.T.);
#14665=ORIENTED_EDGE('',*,*,#10121,.F.);
#14666=ORIENTED_EDGE('',*,*,#10116,.T.);
#14667=ORIENTED_EDGE('',*,*,#10117,.T.);
#14668=ORIENTED_EDGE('',*,*,#10124,.T.);
#14669=ORIENTED_EDGE('',*,*,#10122,.F.);
#14670=ORIENTED_EDGE('',*,*,#10123,.F.);
#14671=ORIENTED_EDGE('',*,*,#10124,.F.);
#14672=ORIENTED_EDGE('',*,*,#10125,.F.);
#14673=ORIENTED_EDGE('',*,*,#10126,.F.);
#14674=ORIENTED_EDGE('',*,*,#10127,.T.);
#14675=ORIENTED_EDGE('',*,*,#10119,.T.);
#14676=ORIENTED_EDGE('',*,*,#10120,.T.);
#14677=ORIENTED_EDGE('',*,*,#10127,.F.);
#14678=ORIENTED_EDGE('',*,*,#10128,.F.);
#14679=ORIENTED_EDGE('',*,*,#10129,.F.);
#14680=ORIENTED_EDGE('',*,*,#10130,.T.);
#14681=ORIENTED_EDGE('',*,*,#10131,.T.);
#14682=ORIENTED_EDGE('',*,*,#10132,.T.);
#14683=ORIENTED_EDGE('',*,*,#10130,.F.);
#14684=ORIENTED_EDGE('',*,*,#10125,.T.);
#14685=ORIENTED_EDGE('',*,*,#10126,.T.);
#14686=ORIENTED_EDGE('',*,*,#10133,.T.);
#14687=ORIENTED_EDGE('',*,*,#10131,.F.);
#14688=ORIENTED_EDGE('',*,*,#10132,.F.);
#14689=ORIENTED_EDGE('',*,*,#10133,.F.);
#14690=ORIENTED_EDGE('',*,*,#10134,.F.);
#14691=ORIENTED_EDGE('',*,*,#10135,.F.);
#14692=ORIENTED_EDGE('',*,*,#10136,.T.);
#14693=ORIENTED_EDGE('',*,*,#10128,.T.);
#14694=ORIENTED_EDGE('',*,*,#10129,.T.);
#14695=ORIENTED_EDGE('',*,*,#10136,.F.);
#14696=ORIENTED_EDGE('',*,*,#10137,.F.);
#14697=ORIENTED_EDGE('',*,*,#10138,.F.);
#14698=ORIENTED_EDGE('',*,*,#10139,.T.);
#14699=ORIENTED_EDGE('',*,*,#10140,.T.);
#14700=ORIENTED_EDGE('',*,*,#10141,.T.);
#14701=ORIENTED_EDGE('',*,*,#10139,.F.);
#14702=ORIENTED_EDGE('',*,*,#10134,.T.);
#14703=ORIENTED_EDGE('',*,*,#10135,.T.);
#14704=ORIENTED_EDGE('',*,*,#10142,.T.);
#14705=ORIENTED_EDGE('',*,*,#10140,.F.);
#14706=ORIENTED_EDGE('',*,*,#10141,.F.);
#14707=ORIENTED_EDGE('',*,*,#10142,.F.);
#14708=ORIENTED_EDGE('',*,*,#10143,.F.);
#14709=ORIENTED_EDGE('',*,*,#10144,.F.);
#14710=ORIENTED_EDGE('',*,*,#10145,.T.);
#14711=ORIENTED_EDGE('',*,*,#10137,.T.);
#14712=ORIENTED_EDGE('',*,*,#10138,.T.);
#14713=ORIENTED_EDGE('',*,*,#10145,.F.);
#14714=ORIENTED_EDGE('',*,*,#10146,.F.);
#14715=ORIENTED_EDGE('',*,*,#10147,.F.);
#14716=ORIENTED_EDGE('',*,*,#10148,.T.);
#14717=ORIENTED_EDGE('',*,*,#10149,.T.);
#14718=ORIENTED_EDGE('',*,*,#10150,.T.);
#14719=ORIENTED_EDGE('',*,*,#10148,.F.);
#14720=ORIENTED_EDGE('',*,*,#10143,.T.);
#14721=ORIENTED_EDGE('',*,*,#10144,.T.);
#14722=ORIENTED_EDGE('',*,*,#10151,.T.);
#14723=ORIENTED_EDGE('',*,*,#10149,.F.);
#14724=ORIENTED_EDGE('',*,*,#10150,.F.);
#14725=ORIENTED_EDGE('',*,*,#10151,.F.);
#14726=ORIENTED_EDGE('',*,*,#10152,.F.);
#14727=ORIENTED_EDGE('',*,*,#10153,.F.);
#14728=ORIENTED_EDGE('',*,*,#10154,.T.);
#14729=ORIENTED_EDGE('',*,*,#10146,.T.);
#14730=ORIENTED_EDGE('',*,*,#10147,.T.);
#14731=ORIENTED_EDGE('',*,*,#10154,.F.);
#14732=ORIENTED_EDGE('',*,*,#10155,.F.);
#14733=ORIENTED_EDGE('',*,*,#10156,.F.);
#14734=ORIENTED_EDGE('',*,*,#10157,.T.);
#14735=ORIENTED_EDGE('',*,*,#10158,.T.);
#14736=ORIENTED_EDGE('',*,*,#10159,.T.);
#14737=ORIENTED_EDGE('',*,*,#10157,.F.);
#14738=ORIENTED_EDGE('',*,*,#10152,.T.);
#14739=ORIENTED_EDGE('',*,*,#10153,.T.);
#14740=ORIENTED_EDGE('',*,*,#10160,.T.);
#14741=ORIENTED_EDGE('',*,*,#10158,.F.);
#14742=ORIENTED_EDGE('',*,*,#10159,.F.);
#14743=ORIENTED_EDGE('',*,*,#10160,.F.);
#14744=ORIENTED_EDGE('',*,*,#10161,.F.);
#14745=ORIENTED_EDGE('',*,*,#10162,.F.);
#14746=ORIENTED_EDGE('',*,*,#10163,.T.);
#14747=ORIENTED_EDGE('',*,*,#10155,.T.);
#14748=ORIENTED_EDGE('',*,*,#10156,.T.);
#14749=ORIENTED_EDGE('',*,*,#10163,.F.);
#14750=ORIENTED_EDGE('',*,*,#10164,.F.);
#14751=ORIENTED_EDGE('',*,*,#10165,.F.);
#14752=ORIENTED_EDGE('',*,*,#10166,.T.);
#14753=ORIENTED_EDGE('',*,*,#10167,.T.);
#14754=ORIENTED_EDGE('',*,*,#10168,.T.);
#14755=ORIENTED_EDGE('',*,*,#10166,.F.);
#14756=ORIENTED_EDGE('',*,*,#10161,.T.);
#14757=ORIENTED_EDGE('',*,*,#10162,.T.);
#14758=ORIENTED_EDGE('',*,*,#10169,.T.);
#14759=ORIENTED_EDGE('',*,*,#10167,.F.);
#14760=ORIENTED_EDGE('',*,*,#10168,.F.);
#14761=ORIENTED_EDGE('',*,*,#10169,.F.);
#14762=ORIENTED_EDGE('',*,*,#10170,.F.);
#14763=ORIENTED_EDGE('',*,*,#10171,.F.);
#14764=ORIENTED_EDGE('',*,*,#10172,.T.);
#14765=ORIENTED_EDGE('',*,*,#10164,.T.);
#14766=ORIENTED_EDGE('',*,*,#10165,.T.);
#14767=ORIENTED_EDGE('',*,*,#10172,.F.);
#14768=ORIENTED_EDGE('',*,*,#10173,.F.);
#14769=ORIENTED_EDGE('',*,*,#10174,.F.);
#14770=ORIENTED_EDGE('',*,*,#10175,.T.);
#14771=ORIENTED_EDGE('',*,*,#10176,.T.);
#14772=ORIENTED_EDGE('',*,*,#10177,.T.);
#14773=ORIENTED_EDGE('',*,*,#10175,.F.);
#14774=ORIENTED_EDGE('',*,*,#10170,.T.);
#14775=ORIENTED_EDGE('',*,*,#10171,.T.);
#14776=ORIENTED_EDGE('',*,*,#10178,.T.);
#14777=ORIENTED_EDGE('',*,*,#10176,.F.);
#14778=ORIENTED_EDGE('',*,*,#10177,.F.);
#14779=ORIENTED_EDGE('',*,*,#10178,.F.);
#14780=ORIENTED_EDGE('',*,*,#10179,.F.);
#14781=ORIENTED_EDGE('',*,*,#10180,.F.);
#14782=ORIENTED_EDGE('',*,*,#10181,.T.);
#14783=ORIENTED_EDGE('',*,*,#10173,.T.);
#14784=ORIENTED_EDGE('',*,*,#10174,.T.);
#14785=ORIENTED_EDGE('',*,*,#10181,.F.);
#14786=ORIENTED_EDGE('',*,*,#10182,.F.);
#14787=ORIENTED_EDGE('',*,*,#10183,.F.);
#14788=ORIENTED_EDGE('',*,*,#10184,.T.);
#14789=ORIENTED_EDGE('',*,*,#10185,.T.);
#14790=ORIENTED_EDGE('',*,*,#10186,.T.);
#14791=ORIENTED_EDGE('',*,*,#10184,.F.);
#14792=ORIENTED_EDGE('',*,*,#10179,.T.);
#14793=ORIENTED_EDGE('',*,*,#10180,.T.);
#14794=ORIENTED_EDGE('',*,*,#10187,.T.);
#14795=ORIENTED_EDGE('',*,*,#10185,.F.);
#14796=ORIENTED_EDGE('',*,*,#10186,.F.);
#14797=ORIENTED_EDGE('',*,*,#10187,.F.);
#14798=ORIENTED_EDGE('',*,*,#10188,.F.);
#14799=ORIENTED_EDGE('',*,*,#10189,.F.);
#14800=ORIENTED_EDGE('',*,*,#10190,.T.);
#14801=ORIENTED_EDGE('',*,*,#10182,.T.);
#14802=ORIENTED_EDGE('',*,*,#10183,.T.);
#14803=ORIENTED_EDGE('',*,*,#10190,.F.);
#14804=ORIENTED_EDGE('',*,*,#10191,.F.);
#14805=ORIENTED_EDGE('',*,*,#10192,.F.);
#14806=ORIENTED_EDGE('',*,*,#10193,.T.);
#14807=ORIENTED_EDGE('',*,*,#10194,.T.);
#14808=ORIENTED_EDGE('',*,*,#10195,.T.);
#14809=ORIENTED_EDGE('',*,*,#10193,.F.);
#14810=ORIENTED_EDGE('',*,*,#10188,.T.);
#14811=ORIENTED_EDGE('',*,*,#10189,.T.);
#14812=ORIENTED_EDGE('',*,*,#10196,.T.);
#14813=ORIENTED_EDGE('',*,*,#10194,.F.);
#14814=ORIENTED_EDGE('',*,*,#10195,.F.);
#14815=ORIENTED_EDGE('',*,*,#10196,.F.);
#14816=ORIENTED_EDGE('',*,*,#10197,.F.);
#14817=ORIENTED_EDGE('',*,*,#10198,.F.);
#14818=ORIENTED_EDGE('',*,*,#10199,.T.);
#14819=ORIENTED_EDGE('',*,*,#10191,.T.);
#14820=ORIENTED_EDGE('',*,*,#10192,.T.);
#14821=ORIENTED_EDGE('',*,*,#10199,.F.);
#14822=ORIENTED_EDGE('',*,*,#10200,.F.);
#14823=ORIENTED_EDGE('',*,*,#10201,.F.);
#14824=ORIENTED_EDGE('',*,*,#10202,.T.);
#14825=ORIENTED_EDGE('',*,*,#10203,.T.);
#14826=ORIENTED_EDGE('',*,*,#10204,.T.);
#14827=ORIENTED_EDGE('',*,*,#10202,.F.);
#14828=ORIENTED_EDGE('',*,*,#10197,.T.);
#14829=ORIENTED_EDGE('',*,*,#10198,.T.);
#14830=ORIENTED_EDGE('',*,*,#10205,.T.);
#14831=ORIENTED_EDGE('',*,*,#10203,.F.);
#14832=ORIENTED_EDGE('',*,*,#10204,.F.);
#14833=ORIENTED_EDGE('',*,*,#10205,.F.);
#14834=ORIENTED_EDGE('',*,*,#10087,.T.);
#14835=ORIENTED_EDGE('',*,*,#10206,.T.);
#14836=ORIENTED_EDGE('',*,*,#10207,.T.);
#14837=ORIENTED_EDGE('',*,*,#10206,.F.);
#14838=ORIENTED_EDGE('',*,*,#10208,.T.);
#14839=ORIENTED_EDGE('',*,*,#10209,.F.);
#14840=ORIENTED_EDGE('',*,*,#10210,.T.);
#14841=ORIENTED_EDGE('',*,*,#10211,.T.);
#14842=ORIENTED_EDGE('',*,*,#10212,.F.);
#14843=ORIENTED_EDGE('',*,*,#10213,.T.);
#14844=ORIENTED_EDGE('',*,*,#10214,.T.);
#14845=ORIENTED_EDGE('',*,*,#10215,.F.);
#14846=ORIENTED_EDGE('',*,*,#10216,.T.);
#14847=ORIENTED_EDGE('',*,*,#10217,.T.);
#14848=ORIENTED_EDGE('',*,*,#10218,.F.);
#14849=ORIENTED_EDGE('',*,*,#10219,.T.);
#14850=ORIENTED_EDGE('',*,*,#10220,.T.);
#14851=ORIENTED_EDGE('',*,*,#10221,.F.);
#14852=ORIENTED_EDGE('',*,*,#10222,.T.);
#14853=ORIENTED_EDGE('',*,*,#10223,.T.);
#14854=ORIENTED_EDGE('',*,*,#10224,.F.);
#14855=ORIENTED_EDGE('',*,*,#10225,.T.);
#14856=ORIENTED_EDGE('',*,*,#10226,.T.);
#14857=ORIENTED_EDGE('',*,*,#10227,.F.);
#14858=ORIENTED_EDGE('',*,*,#10228,.T.);
#14859=ORIENTED_EDGE('',*,*,#10229,.T.);
#14860=ORIENTED_EDGE('',*,*,#10230,.F.);
#14861=ORIENTED_EDGE('',*,*,#10231,.T.);
#14862=ORIENTED_EDGE('',*,*,#10232,.T.);
#14863=ORIENTED_EDGE('',*,*,#10233,.F.);
#14864=ORIENTED_EDGE('',*,*,#10234,.T.);
#14865=ORIENTED_EDGE('',*,*,#10235,.T.);
#14866=ORIENTED_EDGE('',*,*,#10236,.F.);
#14867=ORIENTED_EDGE('',*,*,#10237,.T.);
#14868=ORIENTED_EDGE('',*,*,#10238,.T.);
#14869=ORIENTED_EDGE('',*,*,#10239,.F.);
#14870=ORIENTED_EDGE('',*,*,#10240,.T.);
#14871=ORIENTED_EDGE('',*,*,#10241,.T.);
#14872=ORIENTED_EDGE('',*,*,#10242,.F.);
#14873=ORIENTED_EDGE('',*,*,#10243,.T.);
#14874=ORIENTED_EDGE('',*,*,#10244,.T.);
#14875=ORIENTED_EDGE('',*,*,#10245,.F.);
#14876=ORIENTED_EDGE('',*,*,#10246,.T.);
#14877=ORIENTED_EDGE('',*,*,#10247,.T.);
#14878=ORIENTED_EDGE('',*,*,#10248,.F.);
#14879=ORIENTED_EDGE('',*,*,#10249,.T.);
#14880=ORIENTED_EDGE('',*,*,#10250,.T.);
#14881=ORIENTED_EDGE('',*,*,#10251,.F.);
#14882=ORIENTED_EDGE('',*,*,#10252,.T.);
#14883=ORIENTED_EDGE('',*,*,#10253,.T.);
#14884=ORIENTED_EDGE('',*,*,#10254,.F.);
#14885=ORIENTED_EDGE('',*,*,#10255,.T.);
#14886=ORIENTED_EDGE('',*,*,#10256,.T.);
#14887=ORIENTED_EDGE('',*,*,#10257,.F.);
#14888=ORIENTED_EDGE('',*,*,#10258,.T.);
#14889=ORIENTED_EDGE('',*,*,#10259,.T.);
#14890=ORIENTED_EDGE('',*,*,#10260,.F.);
#14891=ORIENTED_EDGE('',*,*,#10261,.T.);
#14892=ORIENTED_EDGE('',*,*,#10262,.T.);
#14893=ORIENTED_EDGE('',*,*,#10263,.F.);
#14894=ORIENTED_EDGE('',*,*,#10264,.T.);
#14895=ORIENTED_EDGE('',*,*,#10265,.T.);
#14896=ORIENTED_EDGE('',*,*,#10266,.F.);
#14897=ORIENTED_EDGE('',*,*,#10267,.T.);
#14898=ORIENTED_EDGE('',*,*,#10268,.T.);
#14899=ORIENTED_EDGE('',*,*,#10269,.F.);
#14900=ORIENTED_EDGE('',*,*,#10270,.T.);
#14901=ORIENTED_EDGE('',*,*,#10271,.T.);
#14902=ORIENTED_EDGE('',*,*,#10272,.F.);
#14903=ORIENTED_EDGE('',*,*,#10273,.T.);
#14904=ORIENTED_EDGE('',*,*,#10274,.T.);
#14905=ORIENTED_EDGE('',*,*,#10275,.F.);
#14906=ORIENTED_EDGE('',*,*,#10276,.T.);
#14907=ORIENTED_EDGE('',*,*,#10277,.T.);
#14908=ORIENTED_EDGE('',*,*,#10278,.F.);
#14909=ORIENTED_EDGE('',*,*,#10279,.T.);
#14910=ORIENTED_EDGE('',*,*,#10280,.T.);
#14911=ORIENTED_EDGE('',*,*,#10281,.F.);
#14912=ORIENTED_EDGE('',*,*,#10282,.T.);
#14913=ORIENTED_EDGE('',*,*,#10283,.T.);
#14914=ORIENTED_EDGE('',*,*,#10284,.F.);
#14915=ORIENTED_EDGE('',*,*,#10285,.T.);
#14916=ORIENTED_EDGE('',*,*,#10286,.T.);
#14917=ORIENTED_EDGE('',*,*,#10287,.F.);
#14918=ORIENTED_EDGE('',*,*,#10288,.T.);
#14919=ORIENTED_EDGE('',*,*,#10289,.T.);
#14920=ORIENTED_EDGE('',*,*,#10290,.F.);
#14921=ORIENTED_EDGE('',*,*,#10291,.T.);
#14922=ORIENTED_EDGE('',*,*,#10292,.T.);
#14923=ORIENTED_EDGE('',*,*,#10293,.F.);
#14924=ORIENTED_EDGE('',*,*,#10294,.T.);
#14925=ORIENTED_EDGE('',*,*,#10295,.T.);
#14926=ORIENTED_EDGE('',*,*,#10296,.F.);
#14927=ORIENTED_EDGE('',*,*,#10297,.T.);
#14928=ORIENTED_EDGE('',*,*,#10298,.T.);
#14929=ORIENTED_EDGE('',*,*,#10299,.F.);
#14930=ORIENTED_EDGE('',*,*,#10300,.T.);
#14931=ORIENTED_EDGE('',*,*,#10301,.T.);
#14932=ORIENTED_EDGE('',*,*,#10302,.F.);
#14933=ORIENTED_EDGE('',*,*,#10303,.T.);
#14934=ORIENTED_EDGE('',*,*,#10304,.T.);
#14935=ORIENTED_EDGE('',*,*,#10305,.F.);
#14936=ORIENTED_EDGE('',*,*,#10306,.T.);
#14937=ORIENTED_EDGE('',*,*,#10307,.T.);
#14938=ORIENTED_EDGE('',*,*,#10308,.F.);
#14939=ORIENTED_EDGE('',*,*,#10309,.T.);
#14940=ORIENTED_EDGE('',*,*,#10310,.T.);
#14941=ORIENTED_EDGE('',*,*,#10311,.F.);
#14942=ORIENTED_EDGE('',*,*,#10312,.T.);
#14943=ORIENTED_EDGE('',*,*,#10313,.T.);
#14944=ORIENTED_EDGE('',*,*,#10314,.F.);
#14945=ORIENTED_EDGE('',*,*,#10315,.T.);
#14946=ORIENTED_EDGE('',*,*,#10316,.T.);
#14947=ORIENTED_EDGE('',*,*,#10317,.F.);
#14948=ORIENTED_EDGE('',*,*,#10318,.T.);
#14949=ORIENTED_EDGE('',*,*,#10319,.T.);
#14950=ORIENTED_EDGE('',*,*,#10320,.F.);
#14951=ORIENTED_EDGE('',*,*,#10321,.T.);
#14952=ORIENTED_EDGE('',*,*,#10322,.T.);
#14953=ORIENTED_EDGE('',*,*,#10323,.F.);
#14954=ORIENTED_EDGE('',*,*,#10324,.T.);
#14955=ORIENTED_EDGE('',*,*,#10325,.T.);
#14956=ORIENTED_EDGE('',*,*,#10326,.T.);
#14957=ORIENTED_EDGE('',*,*,#10325,.F.);
#14958=ORIENTED_EDGE('',*,*,#10327,.T.);
#14959=ORIENTED_EDGE('',*,*,#10328,.T.);
#14960=ORIENTED_EDGE('',*,*,#10329,.F.);
#14961=ORIENTED_EDGE('',*,*,#10330,.T.);
#14962=ORIENTED_EDGE('',*,*,#10331,.T.);
#14963=ORIENTED_EDGE('',*,*,#10332,.F.);
#14964=ORIENTED_EDGE('',*,*,#10333,.T.);
#14965=ORIENTED_EDGE('',*,*,#10334,.T.);
#14966=ORIENTED_EDGE('',*,*,#10335,.F.);
#14967=ORIENTED_EDGE('',*,*,#10336,.T.);
#14968=ORIENTED_EDGE('',*,*,#10337,.T.);
#14969=ORIENTED_EDGE('',*,*,#10338,.F.);
#14970=ORIENTED_EDGE('',*,*,#10339,.T.);
#14971=ORIENTED_EDGE('',*,*,#10340,.T.);
#14972=ORIENTED_EDGE('',*,*,#10341,.F.);
#14973=ORIENTED_EDGE('',*,*,#10342,.T.);
#14974=ORIENTED_EDGE('',*,*,#10343,.T.);
#14975=ORIENTED_EDGE('',*,*,#10344,.F.);
#14976=ORIENTED_EDGE('',*,*,#10345,.T.);
#14977=ORIENTED_EDGE('',*,*,#10346,.T.);
#14978=ORIENTED_EDGE('',*,*,#10347,.F.);
#14979=ORIENTED_EDGE('',*,*,#10348,.T.);
#14980=ORIENTED_EDGE('',*,*,#10349,.T.);
#14981=ORIENTED_EDGE('',*,*,#10350,.F.);
#14982=ORIENTED_EDGE('',*,*,#10351,.T.);
#14983=ORIENTED_EDGE('',*,*,#10352,.T.);
#14984=ORIENTED_EDGE('',*,*,#10353,.F.);
#14985=ORIENTED_EDGE('',*,*,#10354,.T.);
#14986=ORIENTED_EDGE('',*,*,#10355,.T.);
#14987=ORIENTED_EDGE('',*,*,#10356,.F.);
#14988=ORIENTED_EDGE('',*,*,#10357,.T.);
#14989=ORIENTED_EDGE('',*,*,#10358,.T.);
#14990=ORIENTED_EDGE('',*,*,#10359,.F.);
#14991=ORIENTED_EDGE('',*,*,#10360,.T.);
#14992=ORIENTED_EDGE('',*,*,#10361,.T.);
#14993=ORIENTED_EDGE('',*,*,#10362,.F.);
#14994=ORIENTED_EDGE('',*,*,#10363,.T.);
#14995=ORIENTED_EDGE('',*,*,#10364,.T.);
#14996=ORIENTED_EDGE('',*,*,#10365,.F.);
#14997=ORIENTED_EDGE('',*,*,#10366,.T.);
#14998=ORIENTED_EDGE('',*,*,#10367,.T.);
#14999=ORIENTED_EDGE('',*,*,#10368,.F.);
#15000=ORIENTED_EDGE('',*,*,#10369,.T.);
#15001=ORIENTED_EDGE('',*,*,#10370,.T.);
#15002=ORIENTED_EDGE('',*,*,#10371,.F.);
#15003=ORIENTED_EDGE('',*,*,#10372,.T.);
#15004=ORIENTED_EDGE('',*,*,#10373,.T.);
#15005=ORIENTED_EDGE('',*,*,#10374,.F.);
#15006=ORIENTED_EDGE('',*,*,#10375,.T.);
#15007=ORIENTED_EDGE('',*,*,#10376,.T.);
#15008=ORIENTED_EDGE('',*,*,#10377,.F.);
#15009=ORIENTED_EDGE('',*,*,#10378,.T.);
#15010=ORIENTED_EDGE('',*,*,#10379,.T.);
#15011=ORIENTED_EDGE('',*,*,#10380,.F.);
#15012=ORIENTED_EDGE('',*,*,#10381,.T.);
#15013=ORIENTED_EDGE('',*,*,#10382,.T.);
#15014=ORIENTED_EDGE('',*,*,#10383,.F.);
#15015=ORIENTED_EDGE('',*,*,#10384,.T.);
#15016=ORIENTED_EDGE('',*,*,#10385,.T.);
#15017=ORIENTED_EDGE('',*,*,#10386,.F.);
#15018=ORIENTED_EDGE('',*,*,#10387,.T.);
#15019=ORIENTED_EDGE('',*,*,#10388,.T.);
#15020=ORIENTED_EDGE('',*,*,#10389,.F.);
#15021=ORIENTED_EDGE('',*,*,#10390,.T.);
#15022=ORIENTED_EDGE('',*,*,#10391,.T.);
#15023=ORIENTED_EDGE('',*,*,#10392,.F.);
#15024=ORIENTED_EDGE('',*,*,#10393,.T.);
#15025=ORIENTED_EDGE('',*,*,#10394,.T.);
#15026=ORIENTED_EDGE('',*,*,#10395,.F.);
#15027=ORIENTED_EDGE('',*,*,#10396,.T.);
#15028=ORIENTED_EDGE('',*,*,#10397,.T.);
#15029=ORIENTED_EDGE('',*,*,#10398,.F.);
#15030=ORIENTED_EDGE('',*,*,#10399,.T.);
#15031=ORIENTED_EDGE('',*,*,#10400,.T.);
#15032=ORIENTED_EDGE('',*,*,#10401,.F.);
#15033=ORIENTED_EDGE('',*,*,#10402,.T.);
#15034=ORIENTED_EDGE('',*,*,#10403,.T.);
#15035=ORIENTED_EDGE('',*,*,#10404,.F.);
#15036=ORIENTED_EDGE('',*,*,#10405,.T.);
#15037=ORIENTED_EDGE('',*,*,#10406,.T.);
#15038=ORIENTED_EDGE('',*,*,#10407,.F.);
#15039=ORIENTED_EDGE('',*,*,#10408,.T.);
#15040=ORIENTED_EDGE('',*,*,#10409,.T.);
#15041=ORIENTED_EDGE('',*,*,#10410,.F.);
#15042=ORIENTED_EDGE('',*,*,#10411,.T.);
#15043=ORIENTED_EDGE('',*,*,#10412,.T.);
#15044=ORIENTED_EDGE('',*,*,#10413,.F.);
#15045=ORIENTED_EDGE('',*,*,#10414,.T.);
#15046=ORIENTED_EDGE('',*,*,#10415,.T.);
#15047=ORIENTED_EDGE('',*,*,#10416,.F.);
#15048=ORIENTED_EDGE('',*,*,#10417,.T.);
#15049=ORIENTED_EDGE('',*,*,#10418,.T.);
#15050=ORIENTED_EDGE('',*,*,#10419,.F.);
#15051=ORIENTED_EDGE('',*,*,#10420,.T.);
#15052=ORIENTED_EDGE('',*,*,#10421,.T.);
#15053=ORIENTED_EDGE('',*,*,#10422,.F.);
#15054=ORIENTED_EDGE('',*,*,#10423,.T.);
#15055=ORIENTED_EDGE('',*,*,#10424,.T.);
#15056=ORIENTED_EDGE('',*,*,#10425,.F.);
#15057=ORIENTED_EDGE('',*,*,#10426,.T.);
#15058=ORIENTED_EDGE('',*,*,#10427,.T.);
#15059=ORIENTED_EDGE('',*,*,#10428,.F.);
#15060=ORIENTED_EDGE('',*,*,#10429,.T.);
#15061=ORIENTED_EDGE('',*,*,#10430,.T.);
#15062=ORIENTED_EDGE('',*,*,#10431,.F.);
#15063=ORIENTED_EDGE('',*,*,#10432,.T.);
#15064=ORIENTED_EDGE('',*,*,#10433,.T.);
#15065=ORIENTED_EDGE('',*,*,#10434,.F.);
#15066=ORIENTED_EDGE('',*,*,#10435,.T.);
#15067=ORIENTED_EDGE('',*,*,#10436,.T.);
#15068=ORIENTED_EDGE('',*,*,#10437,.F.);
#15069=ORIENTED_EDGE('',*,*,#10438,.T.);
#15070=ORIENTED_EDGE('',*,*,#10439,.T.);
#15071=ORIENTED_EDGE('',*,*,#10440,.F.);
#15072=ORIENTED_EDGE('',*,*,#10441,.T.);
#15073=ORIENTED_EDGE('',*,*,#10442,.F.);
#15074=ORIENTED_EDGE('',*,*,#10443,.T.);
#15075=ORIENTED_EDGE('',*,*,#10444,.F.);
#15076=ORIENTED_EDGE('',*,*,#10445,.F.);
#15077=ORIENTED_EDGE('',*,*,#10446,.T.);
#15078=ORIENTED_EDGE('',*,*,#10447,.F.);
#15079=ORIENTED_EDGE('',*,*,#10448,.F.);
#15080=ORIENTED_EDGE('',*,*,#10449,.T.);
#15081=ORIENTED_EDGE('',*,*,#10450,.F.);
#15082=ORIENTED_EDGE('',*,*,#10451,.F.);
#15083=ORIENTED_EDGE('',*,*,#10452,.T.);
#15084=ORIENTED_EDGE('',*,*,#10453,.F.);
#15085=ORIENTED_EDGE('',*,*,#10454,.F.);
#15086=ORIENTED_EDGE('',*,*,#10455,.T.);
#15087=ORIENTED_EDGE('',*,*,#10456,.F.);
#15088=ORIENTED_EDGE('',*,*,#10457,.F.);
#15089=ORIENTED_EDGE('',*,*,#10458,.T.);
#15090=ORIENTED_EDGE('',*,*,#10459,.F.);
#15091=ORIENTED_EDGE('',*,*,#10460,.F.);
#15092=ORIENTED_EDGE('',*,*,#10461,.T.);
#15093=ORIENTED_EDGE('',*,*,#10462,.F.);
#15094=ORIENTED_EDGE('',*,*,#10463,.F.);
#15095=ORIENTED_EDGE('',*,*,#10464,.T.);
#15096=ORIENTED_EDGE('',*,*,#10465,.F.);
#15097=ORIENTED_EDGE('',*,*,#10466,.F.);
#15098=ORIENTED_EDGE('',*,*,#10467,.T.);
#15099=ORIENTED_EDGE('',*,*,#10468,.F.);
#15100=ORIENTED_EDGE('',*,*,#10469,.F.);
#15101=ORIENTED_EDGE('',*,*,#10470,.T.);
#15102=ORIENTED_EDGE('',*,*,#10471,.F.);
#15103=ORIENTED_EDGE('',*,*,#10472,.F.);
#15104=ORIENTED_EDGE('',*,*,#10473,.T.);
#15105=ORIENTED_EDGE('',*,*,#10474,.F.);
#15106=ORIENTED_EDGE('',*,*,#10475,.F.);
#15107=ORIENTED_EDGE('',*,*,#10476,.T.);
#15108=ORIENTED_EDGE('',*,*,#10477,.F.);
#15109=ORIENTED_EDGE('',*,*,#10478,.F.);
#15110=ORIENTED_EDGE('',*,*,#10479,.T.);
#15111=ORIENTED_EDGE('',*,*,#10480,.F.);
#15112=ORIENTED_EDGE('',*,*,#10481,.F.);
#15113=ORIENTED_EDGE('',*,*,#10482,.T.);
#15114=ORIENTED_EDGE('',*,*,#10483,.F.);
#15115=ORIENTED_EDGE('',*,*,#10484,.F.);
#15116=ORIENTED_EDGE('',*,*,#10485,.T.);
#15117=ORIENTED_EDGE('',*,*,#10486,.F.);
#15118=ORIENTED_EDGE('',*,*,#10487,.F.);
#15119=ORIENTED_EDGE('',*,*,#10488,.T.);
#15120=ORIENTED_EDGE('',*,*,#10489,.F.);
#15121=ORIENTED_EDGE('',*,*,#10490,.F.);
#15122=ORIENTED_EDGE('',*,*,#10491,.T.);
#15123=ORIENTED_EDGE('',*,*,#10492,.F.);
#15124=ORIENTED_EDGE('',*,*,#10493,.F.);
#15125=ORIENTED_EDGE('',*,*,#10494,.T.);
#15126=ORIENTED_EDGE('',*,*,#10495,.F.);
#15127=ORIENTED_EDGE('',*,*,#10496,.F.);
#15128=ORIENTED_EDGE('',*,*,#10497,.T.);
#15129=ORIENTED_EDGE('',*,*,#10498,.F.);
#15130=ORIENTED_EDGE('',*,*,#10499,.F.);
#15131=ORIENTED_EDGE('',*,*,#10500,.T.);
#15132=ORIENTED_EDGE('',*,*,#10501,.F.);
#15133=ORIENTED_EDGE('',*,*,#10502,.F.);
#15134=ORIENTED_EDGE('',*,*,#10503,.T.);
#15135=ORIENTED_EDGE('',*,*,#10504,.F.);
#15136=ORIENTED_EDGE('',*,*,#10505,.F.);
#15137=ORIENTED_EDGE('',*,*,#10506,.T.);
#15138=ORIENTED_EDGE('',*,*,#10507,.F.);
#15139=ORIENTED_EDGE('',*,*,#10508,.F.);
#15140=ORIENTED_EDGE('',*,*,#10509,.T.);
#15141=ORIENTED_EDGE('',*,*,#10510,.F.);
#15142=ORIENTED_EDGE('',*,*,#10511,.F.);
#15143=ORIENTED_EDGE('',*,*,#10512,.T.);
#15144=ORIENTED_EDGE('',*,*,#10513,.F.);
#15145=ORIENTED_EDGE('',*,*,#10514,.F.);
#15146=ORIENTED_EDGE('',*,*,#10515,.T.);
#15147=ORIENTED_EDGE('',*,*,#10516,.F.);
#15148=ORIENTED_EDGE('',*,*,#10517,.F.);
#15149=ORIENTED_EDGE('',*,*,#10518,.T.);
#15150=ORIENTED_EDGE('',*,*,#10519,.F.);
#15151=ORIENTED_EDGE('',*,*,#10520,.F.);
#15152=ORIENTED_EDGE('',*,*,#10521,.T.);
#15153=ORIENTED_EDGE('',*,*,#10522,.F.);
#15154=ORIENTED_EDGE('',*,*,#10523,.F.);
#15155=ORIENTED_EDGE('',*,*,#10524,.T.);
#15156=ORIENTED_EDGE('',*,*,#10525,.F.);
#15157=ORIENTED_EDGE('',*,*,#10526,.F.);
#15158=ORIENTED_EDGE('',*,*,#10527,.T.);
#15159=ORIENTED_EDGE('',*,*,#10528,.F.);
#15160=ORIENTED_EDGE('',*,*,#10529,.F.);
#15161=ORIENTED_EDGE('',*,*,#10530,.T.);
#15162=ORIENTED_EDGE('',*,*,#10531,.F.);
#15163=ORIENTED_EDGE('',*,*,#10532,.F.);
#15164=ORIENTED_EDGE('',*,*,#10533,.T.);
#15165=ORIENTED_EDGE('',*,*,#10534,.F.);
#15166=ORIENTED_EDGE('',*,*,#10535,.F.);
#15167=ORIENTED_EDGE('',*,*,#10536,.T.);
#15168=ORIENTED_EDGE('',*,*,#10537,.F.);
#15169=ORIENTED_EDGE('',*,*,#10538,.F.);
#15170=ORIENTED_EDGE('',*,*,#10539,.T.);
#15171=ORIENTED_EDGE('',*,*,#10540,.F.);
#15172=ORIENTED_EDGE('',*,*,#10541,.F.);
#15173=ORIENTED_EDGE('',*,*,#10542,.T.);
#15174=ORIENTED_EDGE('',*,*,#10543,.F.);
#15175=ORIENTED_EDGE('',*,*,#10544,.F.);
#15176=ORIENTED_EDGE('',*,*,#10545,.T.);
#15177=ORIENTED_EDGE('',*,*,#10546,.F.);
#15178=ORIENTED_EDGE('',*,*,#10547,.F.);
#15179=ORIENTED_EDGE('',*,*,#10548,.T.);
#15180=ORIENTED_EDGE('',*,*,#10549,.F.);
#15181=ORIENTED_EDGE('',*,*,#10550,.F.);
#15182=ORIENTED_EDGE('',*,*,#10551,.T.);
#15183=ORIENTED_EDGE('',*,*,#10552,.F.);
#15184=ORIENTED_EDGE('',*,*,#10553,.F.);
#15185=ORIENTED_EDGE('',*,*,#10554,.T.);
#15186=ORIENTED_EDGE('',*,*,#10555,.F.);
#15187=ORIENTED_EDGE('',*,*,#10556,.F.);
#15188=ORIENTED_EDGE('',*,*,#10557,.T.);
#15189=ORIENTED_EDGE('',*,*,#10558,.F.);
#15190=ORIENTED_EDGE('',*,*,#10559,.T.);
#15191=ORIENTED_EDGE('',*,*,#10560,.F.);
#15192=ORIENTED_EDGE('',*,*,#10559,.F.);
#15193=ORIENTED_EDGE('',*,*,#10561,.F.);
#15194=ORIENTED_EDGE('',*,*,#10562,.F.);
#15195=ORIENTED_EDGE('',*,*,#10563,.T.);
#15196=ORIENTED_EDGE('',*,*,#10564,.F.);
#15197=ORIENTED_EDGE('',*,*,#10565,.F.);
#15198=ORIENTED_EDGE('',*,*,#10566,.T.);
#15199=ORIENTED_EDGE('',*,*,#10567,.F.);
#15200=ORIENTED_EDGE('',*,*,#10568,.F.);
#15201=ORIENTED_EDGE('',*,*,#10569,.T.);
#15202=ORIENTED_EDGE('',*,*,#10570,.F.);
#15203=ORIENTED_EDGE('',*,*,#10571,.F.);
#15204=ORIENTED_EDGE('',*,*,#10572,.T.);
#15205=ORIENTED_EDGE('',*,*,#10573,.F.);
#15206=ORIENTED_EDGE('',*,*,#10574,.F.);
#15207=ORIENTED_EDGE('',*,*,#10575,.T.);
#15208=ORIENTED_EDGE('',*,*,#10576,.F.);
#15209=ORIENTED_EDGE('',*,*,#10577,.F.);
#15210=ORIENTED_EDGE('',*,*,#10578,.T.);
#15211=ORIENTED_EDGE('',*,*,#10579,.F.);
#15212=ORIENTED_EDGE('',*,*,#10580,.F.);
#15213=ORIENTED_EDGE('',*,*,#10581,.T.);
#15214=ORIENTED_EDGE('',*,*,#10582,.F.);
#15215=ORIENTED_EDGE('',*,*,#10583,.F.);
#15216=ORIENTED_EDGE('',*,*,#10584,.T.);
#15217=ORIENTED_EDGE('',*,*,#10585,.F.);
#15218=ORIENTED_EDGE('',*,*,#10586,.F.);
#15219=ORIENTED_EDGE('',*,*,#10587,.T.);
#15220=ORIENTED_EDGE('',*,*,#10588,.F.);
#15221=ORIENTED_EDGE('',*,*,#10589,.F.);
#15222=ORIENTED_EDGE('',*,*,#10590,.T.);
#15223=ORIENTED_EDGE('',*,*,#10591,.F.);
#15224=ORIENTED_EDGE('',*,*,#10592,.F.);
#15225=ORIENTED_EDGE('',*,*,#10593,.T.);
#15226=ORIENTED_EDGE('',*,*,#10594,.F.);
#15227=ORIENTED_EDGE('',*,*,#10595,.F.);
#15228=ORIENTED_EDGE('',*,*,#10596,.T.);
#15229=ORIENTED_EDGE('',*,*,#10597,.F.);
#15230=ORIENTED_EDGE('',*,*,#10598,.F.);
#15231=ORIENTED_EDGE('',*,*,#10599,.T.);
#15232=ORIENTED_EDGE('',*,*,#10600,.F.);
#15233=ORIENTED_EDGE('',*,*,#10601,.F.);
#15234=ORIENTED_EDGE('',*,*,#10602,.T.);
#15235=ORIENTED_EDGE('',*,*,#10603,.F.);
#15236=ORIENTED_EDGE('',*,*,#10604,.F.);
#15237=ORIENTED_EDGE('',*,*,#10605,.T.);
#15238=ORIENTED_EDGE('',*,*,#10606,.F.);
#15239=ORIENTED_EDGE('',*,*,#10607,.F.);
#15240=ORIENTED_EDGE('',*,*,#10608,.T.);
#15241=ORIENTED_EDGE('',*,*,#10609,.F.);
#15242=ORIENTED_EDGE('',*,*,#10610,.F.);
#15243=ORIENTED_EDGE('',*,*,#10611,.T.);
#15244=ORIENTED_EDGE('',*,*,#10612,.F.);
#15245=ORIENTED_EDGE('',*,*,#10613,.F.);
#15246=ORIENTED_EDGE('',*,*,#10614,.T.);
#15247=ORIENTED_EDGE('',*,*,#10615,.F.);
#15248=ORIENTED_EDGE('',*,*,#10616,.F.);
#15249=ORIENTED_EDGE('',*,*,#10617,.T.);
#15250=ORIENTED_EDGE('',*,*,#10618,.F.);
#15251=ORIENTED_EDGE('',*,*,#10619,.F.);
#15252=ORIENTED_EDGE('',*,*,#10620,.T.);
#15253=ORIENTED_EDGE('',*,*,#10621,.F.);
#15254=ORIENTED_EDGE('',*,*,#10622,.F.);
#15255=ORIENTED_EDGE('',*,*,#10623,.T.);
#15256=ORIENTED_EDGE('',*,*,#10624,.F.);
#15257=ORIENTED_EDGE('',*,*,#10625,.F.);
#15258=ORIENTED_EDGE('',*,*,#10626,.T.);
#15259=ORIENTED_EDGE('',*,*,#10627,.F.);
#15260=ORIENTED_EDGE('',*,*,#10628,.F.);
#15261=ORIENTED_EDGE('',*,*,#10629,.T.);
#15262=ORIENTED_EDGE('',*,*,#10630,.F.);
#15263=ORIENTED_EDGE('',*,*,#10631,.F.);
#15264=ORIENTED_EDGE('',*,*,#10632,.T.);
#15265=ORIENTED_EDGE('',*,*,#10633,.F.);
#15266=ORIENTED_EDGE('',*,*,#10634,.F.);
#15267=ORIENTED_EDGE('',*,*,#10635,.T.);
#15268=ORIENTED_EDGE('',*,*,#10636,.F.);
#15269=ORIENTED_EDGE('',*,*,#10637,.F.);
#15270=ORIENTED_EDGE('',*,*,#10638,.T.);
#15271=ORIENTED_EDGE('',*,*,#10639,.F.);
#15272=ORIENTED_EDGE('',*,*,#10640,.F.);
#15273=ORIENTED_EDGE('',*,*,#10641,.T.);
#15274=ORIENTED_EDGE('',*,*,#10642,.F.);
#15275=ORIENTED_EDGE('',*,*,#10643,.F.);
#15276=ORIENTED_EDGE('',*,*,#10644,.T.);
#15277=ORIENTED_EDGE('',*,*,#10645,.F.);
#15278=ORIENTED_EDGE('',*,*,#10646,.F.);
#15279=ORIENTED_EDGE('',*,*,#10647,.T.);
#15280=ORIENTED_EDGE('',*,*,#10648,.F.);
#15281=ORIENTED_EDGE('',*,*,#10649,.F.);
#15282=ORIENTED_EDGE('',*,*,#10650,.T.);
#15283=ORIENTED_EDGE('',*,*,#10651,.F.);
#15284=ORIENTED_EDGE('',*,*,#10652,.F.);
#15285=ORIENTED_EDGE('',*,*,#10653,.T.);
#15286=ORIENTED_EDGE('',*,*,#10654,.F.);
#15287=ORIENTED_EDGE('',*,*,#10655,.F.);
#15288=ORIENTED_EDGE('',*,*,#10656,.T.);
#15289=ORIENTED_EDGE('',*,*,#10657,.F.);
#15290=ORIENTED_EDGE('',*,*,#10658,.F.);
#15291=ORIENTED_EDGE('',*,*,#10659,.T.);
#15292=ORIENTED_EDGE('',*,*,#10660,.F.);
#15293=ORIENTED_EDGE('',*,*,#10661,.F.);
#15294=ORIENTED_EDGE('',*,*,#10662,.T.);
#15295=ORIENTED_EDGE('',*,*,#10663,.F.);
#15296=ORIENTED_EDGE('',*,*,#10664,.F.);
#15297=ORIENTED_EDGE('',*,*,#10665,.T.);
#15298=ORIENTED_EDGE('',*,*,#10666,.F.);
#15299=ORIENTED_EDGE('',*,*,#10667,.F.);
#15300=ORIENTED_EDGE('',*,*,#10668,.T.);
#15301=ORIENTED_EDGE('',*,*,#10669,.F.);
#15302=ORIENTED_EDGE('',*,*,#10670,.F.);
#15303=ORIENTED_EDGE('',*,*,#10671,.T.);
#15304=ORIENTED_EDGE('',*,*,#10672,.F.);
#15305=ORIENTED_EDGE('',*,*,#10673,.F.);
#15306=ORIENTED_EDGE('',*,*,#10674,.T.);
#15307=ORIENTED_EDGE('',*,*,#10675,.F.);
#15308=ORIENTED_EDGE('',*,*,#10676,.F.);
#15309=ORIENTED_EDGE('',*,*,#10677,.T.);
#15310=ORIENTED_EDGE('',*,*,#10200,.T.);
#15311=ORIENTED_EDGE('',*,*,#10201,.T.);
#15312=ORIENTED_EDGE('',*,*,#10677,.F.);
#15313=ORIENTED_EDGE('',*,*,#10678,.F.);
#15314=ORIENTED_EDGE('',*,*,#10389,.T.);
#15315=ORIENTED_EDGE('',*,*,#10679,.T.);
#15316=ORIENTED_EDGE('',*,*,#10614,.F.);
#15317=ORIENTED_EDGE('',*,*,#10680,.T.);
#15318=ORIENTED_EDGE('',*,*,#10611,.F.);
#15319=ORIENTED_EDGE('',*,*,#10681,.F.);
#15320=ORIENTED_EDGE('',*,*,#10392,.T.);
#15321=ORIENTED_EDGE('',*,*,#10682,.T.);
#15322=ORIENTED_EDGE('',*,*,#10608,.F.);
#15323=ORIENTED_EDGE('',*,*,#10683,.F.);
#15324=ORIENTED_EDGE('',*,*,#10395,.T.);
#15325=ORIENTED_EDGE('',*,*,#10684,.T.);
#15326=ORIENTED_EDGE('',*,*,#10605,.F.);
#15327=ORIENTED_EDGE('',*,*,#10685,.F.);
#15328=ORIENTED_EDGE('',*,*,#10398,.T.);
#15329=ORIENTED_EDGE('',*,*,#10686,.T.);
#15330=ORIENTED_EDGE('',*,*,#10602,.F.);
#15331=ORIENTED_EDGE('',*,*,#10687,.F.);
#15332=ORIENTED_EDGE('',*,*,#10401,.T.);
#15333=ORIENTED_EDGE('',*,*,#10688,.T.);
#15334=ORIENTED_EDGE('',*,*,#10599,.F.);
#15335=ORIENTED_EDGE('',*,*,#10689,.F.);
#15336=ORIENTED_EDGE('',*,*,#10404,.T.);
#15337=ORIENTED_EDGE('',*,*,#10690,.T.);
#15338=ORIENTED_EDGE('',*,*,#10596,.F.);
#15339=ORIENTED_EDGE('',*,*,#10691,.F.);
#15340=ORIENTED_EDGE('',*,*,#10407,.T.);
#15341=ORIENTED_EDGE('',*,*,#10692,.T.);
#15342=ORIENTED_EDGE('',*,*,#10593,.F.);
#15343=ORIENTED_EDGE('',*,*,#10693,.F.);
#15344=ORIENTED_EDGE('',*,*,#10410,.T.);
#15345=ORIENTED_EDGE('',*,*,#10694,.T.);
#15346=ORIENTED_EDGE('',*,*,#10590,.F.);
#15347=ORIENTED_EDGE('',*,*,#10695,.F.);
#15348=ORIENTED_EDGE('',*,*,#10413,.T.);
#15349=ORIENTED_EDGE('',*,*,#10696,.T.);
#15350=ORIENTED_EDGE('',*,*,#10587,.F.);
#15351=ORIENTED_EDGE('',*,*,#10697,.F.);
#15352=ORIENTED_EDGE('',*,*,#10416,.T.);
#15353=ORIENTED_EDGE('',*,*,#10698,.T.);
#15354=ORIENTED_EDGE('',*,*,#10584,.F.);
#15355=ORIENTED_EDGE('',*,*,#10699,.F.);
#15356=ORIENTED_EDGE('',*,*,#10419,.T.);
#15357=ORIENTED_EDGE('',*,*,#10700,.T.);
#15358=ORIENTED_EDGE('',*,*,#10581,.F.);
#15359=ORIENTED_EDGE('',*,*,#10701,.F.);
#15360=ORIENTED_EDGE('',*,*,#10422,.T.);
#15361=ORIENTED_EDGE('',*,*,#10702,.T.);
#15362=ORIENTED_EDGE('',*,*,#10578,.F.);
#15363=ORIENTED_EDGE('',*,*,#10703,.F.);
#15364=ORIENTED_EDGE('',*,*,#10425,.T.);
#15365=ORIENTED_EDGE('',*,*,#10704,.T.);
#15366=ORIENTED_EDGE('',*,*,#10575,.F.);
#15367=ORIENTED_EDGE('',*,*,#10705,.F.);
#15368=ORIENTED_EDGE('',*,*,#10428,.T.);
#15369=ORIENTED_EDGE('',*,*,#10706,.T.);
#15370=ORIENTED_EDGE('',*,*,#10572,.F.);
#15371=ORIENTED_EDGE('',*,*,#10707,.F.);
#15372=ORIENTED_EDGE('',*,*,#10431,.T.);
#15373=ORIENTED_EDGE('',*,*,#10708,.T.);
#15374=ORIENTED_EDGE('',*,*,#10569,.F.);
#15375=ORIENTED_EDGE('',*,*,#10709,.F.);
#15376=ORIENTED_EDGE('',*,*,#10434,.T.);
#15377=ORIENTED_EDGE('',*,*,#10710,.T.);
#15378=ORIENTED_EDGE('',*,*,#10566,.F.);
#15379=ORIENTED_EDGE('',*,*,#10711,.F.);
#15380=ORIENTED_EDGE('',*,*,#10437,.T.);
#15381=ORIENTED_EDGE('',*,*,#10712,.T.);
#15382=ORIENTED_EDGE('',*,*,#10563,.F.);
#15383=ORIENTED_EDGE('',*,*,#10713,.F.);
#15384=ORIENTED_EDGE('',*,*,#10440,.T.);
#15385=ORIENTED_EDGE('',*,*,#10714,.T.);
#15386=ORIENTED_EDGE('',*,*,#10557,.F.);
#15387=ORIENTED_EDGE('',*,*,#10715,.F.);
#15388=ORIENTED_EDGE('',*,*,#10209,.T.);
#15389=ORIENTED_EDGE('',*,*,#10716,.T.);
#15390=ORIENTED_EDGE('',*,*,#10554,.F.);
#15391=ORIENTED_EDGE('',*,*,#10717,.F.);
#15392=ORIENTED_EDGE('',*,*,#10212,.T.);
#15393=ORIENTED_EDGE('',*,*,#10718,.T.);
#15394=ORIENTED_EDGE('',*,*,#10551,.F.);
#15395=ORIENTED_EDGE('',*,*,#10719,.F.);
#15396=ORIENTED_EDGE('',*,*,#10215,.T.);
#15397=ORIENTED_EDGE('',*,*,#10720,.T.);
#15398=ORIENTED_EDGE('',*,*,#10548,.F.);
#15399=ORIENTED_EDGE('',*,*,#10721,.F.);
#15400=ORIENTED_EDGE('',*,*,#10218,.T.);
#15401=ORIENTED_EDGE('',*,*,#10722,.T.);
#15402=ORIENTED_EDGE('',*,*,#10545,.F.);
#15403=ORIENTED_EDGE('',*,*,#10723,.F.);
#15404=ORIENTED_EDGE('',*,*,#10221,.T.);
#15405=ORIENTED_EDGE('',*,*,#10724,.T.);
#15406=ORIENTED_EDGE('',*,*,#10542,.F.);
#15407=ORIENTED_EDGE('',*,*,#10725,.F.);
#15408=ORIENTED_EDGE('',*,*,#10224,.T.);
#15409=ORIENTED_EDGE('',*,*,#10726,.T.);
#15410=ORIENTED_EDGE('',*,*,#10539,.F.);
#15411=ORIENTED_EDGE('',*,*,#10727,.F.);
#15412=ORIENTED_EDGE('',*,*,#10227,.T.);
#15413=ORIENTED_EDGE('',*,*,#10728,.T.);
#15414=ORIENTED_EDGE('',*,*,#10536,.F.);
#15415=ORIENTED_EDGE('',*,*,#10729,.F.);
#15416=ORIENTED_EDGE('',*,*,#10230,.T.);
#15417=ORIENTED_EDGE('',*,*,#10730,.T.);
#15418=ORIENTED_EDGE('',*,*,#10533,.F.);
#15419=ORIENTED_EDGE('',*,*,#10731,.F.);
#15420=ORIENTED_EDGE('',*,*,#10233,.T.);
#15421=ORIENTED_EDGE('',*,*,#10732,.T.);
#15422=ORIENTED_EDGE('',*,*,#10530,.F.);
#15423=ORIENTED_EDGE('',*,*,#10733,.F.);
#15424=ORIENTED_EDGE('',*,*,#10236,.T.);
#15425=ORIENTED_EDGE('',*,*,#10734,.T.);
#15426=ORIENTED_EDGE('',*,*,#10527,.F.);
#15427=ORIENTED_EDGE('',*,*,#10735,.F.);
#15428=ORIENTED_EDGE('',*,*,#10239,.T.);
#15429=ORIENTED_EDGE('',*,*,#10736,.T.);
#15430=ORIENTED_EDGE('',*,*,#10524,.F.);
#15431=ORIENTED_EDGE('',*,*,#10737,.F.);
#15432=ORIENTED_EDGE('',*,*,#10242,.T.);
#15433=ORIENTED_EDGE('',*,*,#10738,.T.);
#15434=ORIENTED_EDGE('',*,*,#10521,.F.);
#15435=ORIENTED_EDGE('',*,*,#10739,.F.);
#15436=ORIENTED_EDGE('',*,*,#10245,.T.);
#15437=ORIENTED_EDGE('',*,*,#10740,.T.);
#15438=ORIENTED_EDGE('',*,*,#10518,.F.);
#15439=ORIENTED_EDGE('',*,*,#10741,.F.);
#15440=ORIENTED_EDGE('',*,*,#10248,.T.);
#15441=ORIENTED_EDGE('',*,*,#10742,.T.);
#15442=ORIENTED_EDGE('',*,*,#10515,.F.);
#15443=ORIENTED_EDGE('',*,*,#10743,.F.);
#15444=ORIENTED_EDGE('',*,*,#10251,.T.);
#15445=ORIENTED_EDGE('',*,*,#10744,.T.);
#15446=ORIENTED_EDGE('',*,*,#10512,.F.);
#15447=ORIENTED_EDGE('',*,*,#10745,.F.);
#15448=ORIENTED_EDGE('',*,*,#10254,.T.);
#15449=ORIENTED_EDGE('',*,*,#10746,.T.);
#15450=ORIENTED_EDGE('',*,*,#10509,.F.);
#15451=ORIENTED_EDGE('',*,*,#10747,.F.);
#15452=ORIENTED_EDGE('',*,*,#10257,.T.);
#15453=ORIENTED_EDGE('',*,*,#10748,.T.);
#15454=ORIENTED_EDGE('',*,*,#10506,.F.);
#15455=ORIENTED_EDGE('',*,*,#10749,.F.);
#15456=ORIENTED_EDGE('',*,*,#10260,.T.);
#15457=ORIENTED_EDGE('',*,*,#10750,.T.);
#15458=ORIENTED_EDGE('',*,*,#10503,.F.);
#15459=ORIENTED_EDGE('',*,*,#10751,.F.);
#15460=ORIENTED_EDGE('',*,*,#10263,.T.);
#15461=ORIENTED_EDGE('',*,*,#10752,.T.);
#15462=ORIENTED_EDGE('',*,*,#10500,.F.);
#15463=ORIENTED_EDGE('',*,*,#10753,.F.);
#15464=ORIENTED_EDGE('',*,*,#10266,.T.);
#15465=ORIENTED_EDGE('',*,*,#10754,.T.);
#15466=ORIENTED_EDGE('',*,*,#10497,.F.);
#15467=ORIENTED_EDGE('',*,*,#10755,.F.);
#15468=ORIENTED_EDGE('',*,*,#10269,.T.);
#15469=ORIENTED_EDGE('',*,*,#10756,.T.);
#15470=ORIENTED_EDGE('',*,*,#10494,.F.);
#15471=ORIENTED_EDGE('',*,*,#10757,.F.);
#15472=ORIENTED_EDGE('',*,*,#10272,.T.);
#15473=ORIENTED_EDGE('',*,*,#10758,.T.);
#15474=ORIENTED_EDGE('',*,*,#10491,.F.);
#15475=ORIENTED_EDGE('',*,*,#10759,.F.);
#15476=ORIENTED_EDGE('',*,*,#10275,.T.);
#15477=ORIENTED_EDGE('',*,*,#10760,.T.);
#15478=ORIENTED_EDGE('',*,*,#10488,.F.);
#15479=ORIENTED_EDGE('',*,*,#10761,.F.);
#15480=ORIENTED_EDGE('',*,*,#10278,.T.);
#15481=ORIENTED_EDGE('',*,*,#10762,.T.);
#15482=ORIENTED_EDGE('',*,*,#10485,.F.);
#15483=ORIENTED_EDGE('',*,*,#10763,.F.);
#15484=ORIENTED_EDGE('',*,*,#10281,.T.);
#15485=ORIENTED_EDGE('',*,*,#10764,.T.);
#15486=ORIENTED_EDGE('',*,*,#10482,.F.);
#15487=ORIENTED_EDGE('',*,*,#10765,.F.);
#15488=ORIENTED_EDGE('',*,*,#10284,.T.);
#15489=ORIENTED_EDGE('',*,*,#10766,.T.);
#15490=ORIENTED_EDGE('',*,*,#10479,.F.);
#15491=ORIENTED_EDGE('',*,*,#10767,.F.);
#15492=ORIENTED_EDGE('',*,*,#10287,.T.);
#15493=ORIENTED_EDGE('',*,*,#10768,.T.);
#15494=ORIENTED_EDGE('',*,*,#10476,.F.);
#15495=ORIENTED_EDGE('',*,*,#10769,.F.);
#15496=ORIENTED_EDGE('',*,*,#10290,.T.);
#15497=ORIENTED_EDGE('',*,*,#10770,.T.);
#15498=ORIENTED_EDGE('',*,*,#10473,.F.);
#15499=ORIENTED_EDGE('',*,*,#10771,.F.);
#15500=ORIENTED_EDGE('',*,*,#10293,.T.);
#15501=ORIENTED_EDGE('',*,*,#10772,.T.);
#15502=ORIENTED_EDGE('',*,*,#10470,.F.);
#15503=ORIENTED_EDGE('',*,*,#10773,.F.);
#15504=ORIENTED_EDGE('',*,*,#10296,.T.);
#15505=ORIENTED_EDGE('',*,*,#10774,.T.);
#15506=ORIENTED_EDGE('',*,*,#10467,.F.);
#15507=ORIENTED_EDGE('',*,*,#10775,.F.);
#15508=ORIENTED_EDGE('',*,*,#10299,.T.);
#15509=ORIENTED_EDGE('',*,*,#10776,.T.);
#15510=ORIENTED_EDGE('',*,*,#10464,.F.);
#15511=ORIENTED_EDGE('',*,*,#10777,.F.);
#15512=ORIENTED_EDGE('',*,*,#10302,.T.);
#15513=ORIENTED_EDGE('',*,*,#10778,.T.);
#15514=ORIENTED_EDGE('',*,*,#10461,.F.);
#15515=ORIENTED_EDGE('',*,*,#10779,.F.);
#15516=ORIENTED_EDGE('',*,*,#10305,.T.);
#15517=ORIENTED_EDGE('',*,*,#10780,.T.);
#15518=ORIENTED_EDGE('',*,*,#10458,.F.);
#15519=ORIENTED_EDGE('',*,*,#10781,.F.);
#15520=ORIENTED_EDGE('',*,*,#10308,.T.);
#15521=ORIENTED_EDGE('',*,*,#10782,.T.);
#15522=ORIENTED_EDGE('',*,*,#10455,.F.);
#15523=ORIENTED_EDGE('',*,*,#10783,.F.);
#15524=ORIENTED_EDGE('',*,*,#10311,.T.);
#15525=ORIENTED_EDGE('',*,*,#10784,.T.);
#15526=ORIENTED_EDGE('',*,*,#10452,.F.);
#15527=ORIENTED_EDGE('',*,*,#10785,.F.);
#15528=ORIENTED_EDGE('',*,*,#10314,.T.);
#15529=ORIENTED_EDGE('',*,*,#10786,.T.);
#15530=ORIENTED_EDGE('',*,*,#10449,.F.);
#15531=ORIENTED_EDGE('',*,*,#10787,.F.);
#15532=ORIENTED_EDGE('',*,*,#10317,.T.);
#15533=ORIENTED_EDGE('',*,*,#10788,.T.);
#15534=ORIENTED_EDGE('',*,*,#10446,.F.);
#15535=ORIENTED_EDGE('',*,*,#10789,.F.);
#15536=ORIENTED_EDGE('',*,*,#10320,.T.);
#15537=ORIENTED_EDGE('',*,*,#10790,.T.);
#15538=ORIENTED_EDGE('',*,*,#10443,.F.);
#15539=ORIENTED_EDGE('',*,*,#10791,.F.);
#15540=ORIENTED_EDGE('',*,*,#10323,.T.);
#15541=ORIENTED_EDGE('',*,*,#10792,.T.);
#15542=ORIENTED_EDGE('',*,*,#10674,.F.);
#15543=ORIENTED_EDGE('',*,*,#10793,.F.);
#15544=ORIENTED_EDGE('',*,*,#10329,.T.);
#15545=ORIENTED_EDGE('',*,*,#10794,.T.);
#15546=ORIENTED_EDGE('',*,*,#10671,.F.);
#15547=ORIENTED_EDGE('',*,*,#10795,.F.);
#15548=ORIENTED_EDGE('',*,*,#10332,.T.);
#15549=ORIENTED_EDGE('',*,*,#10796,.T.);
#15550=ORIENTED_EDGE('',*,*,#10668,.F.);
#15551=ORIENTED_EDGE('',*,*,#10797,.F.);
#15552=ORIENTED_EDGE('',*,*,#10335,.T.);
#15553=ORIENTED_EDGE('',*,*,#10798,.T.);
#15554=ORIENTED_EDGE('',*,*,#10665,.F.);
#15555=ORIENTED_EDGE('',*,*,#10799,.F.);
#15556=ORIENTED_EDGE('',*,*,#10338,.T.);
#15557=ORIENTED_EDGE('',*,*,#10800,.T.);
#15558=ORIENTED_EDGE('',*,*,#10662,.F.);
#15559=ORIENTED_EDGE('',*,*,#10801,.F.);
#15560=ORIENTED_EDGE('',*,*,#10341,.T.);
#15561=ORIENTED_EDGE('',*,*,#10802,.T.);
#15562=ORIENTED_EDGE('',*,*,#10659,.F.);
#15563=ORIENTED_EDGE('',*,*,#10803,.F.);
#15564=ORIENTED_EDGE('',*,*,#10344,.T.);
#15565=ORIENTED_EDGE('',*,*,#10804,.T.);
#15566=ORIENTED_EDGE('',*,*,#10656,.F.);
#15567=ORIENTED_EDGE('',*,*,#10805,.F.);
#15568=ORIENTED_EDGE('',*,*,#10347,.T.);
#15569=ORIENTED_EDGE('',*,*,#10806,.T.);
#15570=ORIENTED_EDGE('',*,*,#10653,.F.);
#15571=ORIENTED_EDGE('',*,*,#10807,.F.);
#15572=ORIENTED_EDGE('',*,*,#10350,.T.);
#15573=ORIENTED_EDGE('',*,*,#10808,.T.);
#15574=ORIENTED_EDGE('',*,*,#10650,.F.);
#15575=ORIENTED_EDGE('',*,*,#10809,.F.);
#15576=ORIENTED_EDGE('',*,*,#10353,.T.);
#15577=ORIENTED_EDGE('',*,*,#10810,.T.);
#15578=ORIENTED_EDGE('',*,*,#10647,.F.);
#15579=ORIENTED_EDGE('',*,*,#10811,.F.);
#15580=ORIENTED_EDGE('',*,*,#10356,.T.);
#15581=ORIENTED_EDGE('',*,*,#10812,.T.);
#15582=ORIENTED_EDGE('',*,*,#10644,.F.);
#15583=ORIENTED_EDGE('',*,*,#10813,.F.);
#15584=ORIENTED_EDGE('',*,*,#10359,.T.);
#15585=ORIENTED_EDGE('',*,*,#10814,.T.);
#15586=ORIENTED_EDGE('',*,*,#10641,.F.);
#15587=ORIENTED_EDGE('',*,*,#10815,.F.);
#15588=ORIENTED_EDGE('',*,*,#10362,.T.);
#15589=ORIENTED_EDGE('',*,*,#10816,.T.);
#15590=ORIENTED_EDGE('',*,*,#10638,.F.);
#15591=ORIENTED_EDGE('',*,*,#10817,.F.);
#15592=ORIENTED_EDGE('',*,*,#10365,.T.);
#15593=ORIENTED_EDGE('',*,*,#10818,.T.);
#15594=ORIENTED_EDGE('',*,*,#10635,.F.);
#15595=ORIENTED_EDGE('',*,*,#10819,.F.);
#15596=ORIENTED_EDGE('',*,*,#10368,.T.);
#15597=ORIENTED_EDGE('',*,*,#10820,.T.);
#15598=ORIENTED_EDGE('',*,*,#10632,.F.);
#15599=ORIENTED_EDGE('',*,*,#10821,.F.);
#15600=ORIENTED_EDGE('',*,*,#10371,.T.);
#15601=ORIENTED_EDGE('',*,*,#10822,.T.);
#15602=ORIENTED_EDGE('',*,*,#10629,.F.);
#15603=ORIENTED_EDGE('',*,*,#10823,.F.);
#15604=ORIENTED_EDGE('',*,*,#10374,.T.);
#15605=ORIENTED_EDGE('',*,*,#10824,.T.);
#15606=ORIENTED_EDGE('',*,*,#10626,.F.);
#15607=ORIENTED_EDGE('',*,*,#10825,.F.);
#15608=ORIENTED_EDGE('',*,*,#10377,.T.);
#15609=ORIENTED_EDGE('',*,*,#10826,.T.);
#15610=ORIENTED_EDGE('',*,*,#10623,.F.);
#15611=ORIENTED_EDGE('',*,*,#10827,.F.);
#15612=ORIENTED_EDGE('',*,*,#10380,.T.);
#15613=ORIENTED_EDGE('',*,*,#10828,.F.);
#15614=ORIENTED_EDGE('',*,*,#10386,.T.);
#15615=ORIENTED_EDGE('',*,*,#10829,.T.);
#15616=ORIENTED_EDGE('',*,*,#10617,.F.);
#15617=ORIENTED_EDGE('',*,*,#10560,.T.);
#15618=ORIENTED_EDGE('',*,*,#10830,.T.);
#15619=ORIENTED_EDGE('',*,*,#10620,.F.);
#15620=ORIENTED_EDGE('',*,*,#10831,.F.);
#15621=ORIENTED_EDGE('',*,*,#10383,.T.);
#15622=ORIENTED_EDGE('',*,*,#10326,.F.);
#15623=ORIENTED_EDGE('',*,*,#10085,.T.);
#15624=ORIENTED_EDGE('',*,*,#10207,.F.);
#15625=ORIENTED_EDGE('',*,*,#10676,.T.);
#15626=ORIENTED_EDGE('',*,*,#10091,.F.);
#15627=ORIENTED_EDGE('',*,*,#10619,.T.);
#15628=ORIENTED_EDGE('',*,*,#10832,.F.);
#15629=ORIENTED_EDGE('',*,*,#10384,.F.);
#15630=ORIENTED_EDGE('',*,*,#10831,.T.);
#15631=ORIENTED_EDGE('',*,*,#10618,.T.);
#15632=ORIENTED_EDGE('',*,*,#10829,.F.);
#15633=ORIENTED_EDGE('',*,*,#10385,.F.);
#15634=ORIENTED_EDGE('',*,*,#10832,.T.);
#15635=ORIENTED_EDGE('',*,*,#10616,.T.);
#15636=ORIENTED_EDGE('',*,*,#10833,.F.);
#15637=ORIENTED_EDGE('',*,*,#10387,.F.);
#15638=ORIENTED_EDGE('',*,*,#10828,.T.);
#15639=ORIENTED_EDGE('',*,*,#10615,.T.);
#15640=ORIENTED_EDGE('',*,*,#10679,.F.);
#15641=ORIENTED_EDGE('',*,*,#10388,.F.);
#15642=ORIENTED_EDGE('',*,*,#10833,.T.);
#15643=ORIENTED_EDGE('',*,*,#10622,.T.);
#15644=ORIENTED_EDGE('',*,*,#10834,.F.);
#15645=ORIENTED_EDGE('',*,*,#10381,.F.);
#15646=ORIENTED_EDGE('',*,*,#10827,.T.);
#15647=ORIENTED_EDGE('',*,*,#10621,.T.);
#15648=ORIENTED_EDGE('',*,*,#10830,.F.);
#15649=ORIENTED_EDGE('',*,*,#10382,.F.);
#15650=ORIENTED_EDGE('',*,*,#10834,.T.);
#15651=ORIENTED_EDGE('',*,*,#10625,.T.);
#15652=ORIENTED_EDGE('',*,*,#10835,.F.);
#15653=ORIENTED_EDGE('',*,*,#10378,.F.);
#15654=ORIENTED_EDGE('',*,*,#10825,.T.);
#15655=ORIENTED_EDGE('',*,*,#10624,.T.);
#15656=ORIENTED_EDGE('',*,*,#10826,.F.);
#15657=ORIENTED_EDGE('',*,*,#10379,.F.);
#15658=ORIENTED_EDGE('',*,*,#10835,.T.);
#15659=ORIENTED_EDGE('',*,*,#10628,.T.);
#15660=ORIENTED_EDGE('',*,*,#10836,.F.);
#15661=ORIENTED_EDGE('',*,*,#10375,.F.);
#15662=ORIENTED_EDGE('',*,*,#10823,.T.);
#15663=ORIENTED_EDGE('',*,*,#10627,.T.);
#15664=ORIENTED_EDGE('',*,*,#10824,.F.);
#15665=ORIENTED_EDGE('',*,*,#10376,.F.);
#15666=ORIENTED_EDGE('',*,*,#10836,.T.);
#15667=ORIENTED_EDGE('',*,*,#10631,.T.);
#15668=ORIENTED_EDGE('',*,*,#10837,.F.);
#15669=ORIENTED_EDGE('',*,*,#10372,.F.);
#15670=ORIENTED_EDGE('',*,*,#10821,.T.);
#15671=ORIENTED_EDGE('',*,*,#10630,.T.);
#15672=ORIENTED_EDGE('',*,*,#10822,.F.);
#15673=ORIENTED_EDGE('',*,*,#10373,.F.);
#15674=ORIENTED_EDGE('',*,*,#10837,.T.);
#15675=ORIENTED_EDGE('',*,*,#10634,.T.);
#15676=ORIENTED_EDGE('',*,*,#10838,.F.);
#15677=ORIENTED_EDGE('',*,*,#10369,.F.);
#15678=ORIENTED_EDGE('',*,*,#10819,.T.);
#15679=ORIENTED_EDGE('',*,*,#10633,.T.);
#15680=ORIENTED_EDGE('',*,*,#10820,.F.);
#15681=ORIENTED_EDGE('',*,*,#10370,.F.);
#15682=ORIENTED_EDGE('',*,*,#10838,.T.);
#15683=ORIENTED_EDGE('',*,*,#10637,.T.);
#15684=ORIENTED_EDGE('',*,*,#10839,.F.);
#15685=ORIENTED_EDGE('',*,*,#10366,.F.);
#15686=ORIENTED_EDGE('',*,*,#10817,.T.);
#15687=ORIENTED_EDGE('',*,*,#10636,.T.);
#15688=ORIENTED_EDGE('',*,*,#10818,.F.);
#15689=ORIENTED_EDGE('',*,*,#10367,.F.);
#15690=ORIENTED_EDGE('',*,*,#10839,.T.);
#15691=ORIENTED_EDGE('',*,*,#10640,.T.);
#15692=ORIENTED_EDGE('',*,*,#10840,.F.);
#15693=ORIENTED_EDGE('',*,*,#10363,.F.);
#15694=ORIENTED_EDGE('',*,*,#10815,.T.);
#15695=ORIENTED_EDGE('',*,*,#10639,.T.);
#15696=ORIENTED_EDGE('',*,*,#10816,.F.);
#15697=ORIENTED_EDGE('',*,*,#10364,.F.);
#15698=ORIENTED_EDGE('',*,*,#10840,.T.);
#15699=ORIENTED_EDGE('',*,*,#10643,.T.);
#15700=ORIENTED_EDGE('',*,*,#10841,.F.);
#15701=ORIENTED_EDGE('',*,*,#10360,.F.);
#15702=ORIENTED_EDGE('',*,*,#10813,.T.);
#15703=ORIENTED_EDGE('',*,*,#10642,.T.);
#15704=ORIENTED_EDGE('',*,*,#10814,.F.);
#15705=ORIENTED_EDGE('',*,*,#10361,.F.);
#15706=ORIENTED_EDGE('',*,*,#10841,.T.);
#15707=ORIENTED_EDGE('',*,*,#10646,.T.);
#15708=ORIENTED_EDGE('',*,*,#10842,.F.);
#15709=ORIENTED_EDGE('',*,*,#10357,.F.);
#15710=ORIENTED_EDGE('',*,*,#10811,.T.);
#15711=ORIENTED_EDGE('',*,*,#10645,.T.);
#15712=ORIENTED_EDGE('',*,*,#10812,.F.);
#15713=ORIENTED_EDGE('',*,*,#10358,.F.);
#15714=ORIENTED_EDGE('',*,*,#10842,.T.);
#15715=ORIENTED_EDGE('',*,*,#10649,.T.);
#15716=ORIENTED_EDGE('',*,*,#10843,.F.);
#15717=ORIENTED_EDGE('',*,*,#10354,.F.);
#15718=ORIENTED_EDGE('',*,*,#10809,.T.);
#15719=ORIENTED_EDGE('',*,*,#10648,.T.);
#15720=ORIENTED_EDGE('',*,*,#10810,.F.);
#15721=ORIENTED_EDGE('',*,*,#10355,.F.);
#15722=ORIENTED_EDGE('',*,*,#10843,.T.);
#15723=ORIENTED_EDGE('',*,*,#10652,.T.);
#15724=ORIENTED_EDGE('',*,*,#10844,.F.);
#15725=ORIENTED_EDGE('',*,*,#10351,.F.);
#15726=ORIENTED_EDGE('',*,*,#10807,.T.);
#15727=ORIENTED_EDGE('',*,*,#10651,.T.);
#15728=ORIENTED_EDGE('',*,*,#10808,.F.);
#15729=ORIENTED_EDGE('',*,*,#10352,.F.);
#15730=ORIENTED_EDGE('',*,*,#10844,.T.);
#15731=ORIENTED_EDGE('',*,*,#10655,.T.);
#15732=ORIENTED_EDGE('',*,*,#10845,.F.);
#15733=ORIENTED_EDGE('',*,*,#10348,.F.);
#15734=ORIENTED_EDGE('',*,*,#10805,.T.);
#15735=ORIENTED_EDGE('',*,*,#10654,.T.);
#15736=ORIENTED_EDGE('',*,*,#10806,.F.);
#15737=ORIENTED_EDGE('',*,*,#10349,.F.);
#15738=ORIENTED_EDGE('',*,*,#10845,.T.);
#15739=ORIENTED_EDGE('',*,*,#10658,.T.);
#15740=ORIENTED_EDGE('',*,*,#10846,.F.);
#15741=ORIENTED_EDGE('',*,*,#10345,.F.);
#15742=ORIENTED_EDGE('',*,*,#10803,.T.);
#15743=ORIENTED_EDGE('',*,*,#10657,.T.);
#15744=ORIENTED_EDGE('',*,*,#10804,.F.);
#15745=ORIENTED_EDGE('',*,*,#10346,.F.);
#15746=ORIENTED_EDGE('',*,*,#10846,.T.);
#15747=ORIENTED_EDGE('',*,*,#10661,.T.);
#15748=ORIENTED_EDGE('',*,*,#10847,.F.);
#15749=ORIENTED_EDGE('',*,*,#10342,.F.);
#15750=ORIENTED_EDGE('',*,*,#10801,.T.);
#15751=ORIENTED_EDGE('',*,*,#10660,.T.);
#15752=ORIENTED_EDGE('',*,*,#10802,.F.);
#15753=ORIENTED_EDGE('',*,*,#10343,.F.);
#15754=ORIENTED_EDGE('',*,*,#10847,.T.);
#15755=ORIENTED_EDGE('',*,*,#10664,.T.);
#15756=ORIENTED_EDGE('',*,*,#10848,.F.);
#15757=ORIENTED_EDGE('',*,*,#10339,.F.);
#15758=ORIENTED_EDGE('',*,*,#10799,.T.);
#15759=ORIENTED_EDGE('',*,*,#10663,.T.);
#15760=ORIENTED_EDGE('',*,*,#10800,.F.);
#15761=ORIENTED_EDGE('',*,*,#10340,.F.);
#15762=ORIENTED_EDGE('',*,*,#10848,.T.);
#15763=ORIENTED_EDGE('',*,*,#10667,.T.);
#15764=ORIENTED_EDGE('',*,*,#10849,.F.);
#15765=ORIENTED_EDGE('',*,*,#10336,.F.);
#15766=ORIENTED_EDGE('',*,*,#10797,.T.);
#15767=ORIENTED_EDGE('',*,*,#10666,.T.);
#15768=ORIENTED_EDGE('',*,*,#10798,.F.);
#15769=ORIENTED_EDGE('',*,*,#10337,.F.);
#15770=ORIENTED_EDGE('',*,*,#10849,.T.);
#15771=ORIENTED_EDGE('',*,*,#10670,.T.);
#15772=ORIENTED_EDGE('',*,*,#10850,.F.);
#15773=ORIENTED_EDGE('',*,*,#10333,.F.);
#15774=ORIENTED_EDGE('',*,*,#10795,.T.);
#15775=ORIENTED_EDGE('',*,*,#10669,.T.);
#15776=ORIENTED_EDGE('',*,*,#10796,.F.);
#15777=ORIENTED_EDGE('',*,*,#10334,.F.);
#15778=ORIENTED_EDGE('',*,*,#10850,.T.);
#15779=ORIENTED_EDGE('',*,*,#10673,.T.);
#15780=ORIENTED_EDGE('',*,*,#10851,.F.);
#15781=ORIENTED_EDGE('',*,*,#10330,.F.);
#15782=ORIENTED_EDGE('',*,*,#10793,.T.);
#15783=ORIENTED_EDGE('',*,*,#10672,.T.);
#15784=ORIENTED_EDGE('',*,*,#10794,.F.);
#15785=ORIENTED_EDGE('',*,*,#10331,.F.);
#15786=ORIENTED_EDGE('',*,*,#10851,.T.);
#15787=ORIENTED_EDGE('',*,*,#10442,.T.);
#15788=ORIENTED_EDGE('',*,*,#10852,.F.);
#15789=ORIENTED_EDGE('',*,*,#10327,.F.);
#15790=ORIENTED_EDGE('',*,*,#10324,.F.);
#15791=ORIENTED_EDGE('',*,*,#10791,.T.);
#15792=ORIENTED_EDGE('',*,*,#10675,.T.);
#15793=ORIENTED_EDGE('',*,*,#10792,.F.);
#15794=ORIENTED_EDGE('',*,*,#10328,.F.);
#15795=ORIENTED_EDGE('',*,*,#10852,.T.);
#15796=ORIENTED_EDGE('',*,*,#10445,.T.);
#15797=ORIENTED_EDGE('',*,*,#10853,.F.);
#15798=ORIENTED_EDGE('',*,*,#10321,.F.);
#15799=ORIENTED_EDGE('',*,*,#10789,.T.);
#15800=ORIENTED_EDGE('',*,*,#10444,.T.);
#15801=ORIENTED_EDGE('',*,*,#10790,.F.);
#15802=ORIENTED_EDGE('',*,*,#10322,.F.);
#15803=ORIENTED_EDGE('',*,*,#10853,.T.);
#15804=ORIENTED_EDGE('',*,*,#10448,.T.);
#15805=ORIENTED_EDGE('',*,*,#10854,.F.);
#15806=ORIENTED_EDGE('',*,*,#10318,.F.);
#15807=ORIENTED_EDGE('',*,*,#10787,.T.);
#15808=ORIENTED_EDGE('',*,*,#10447,.T.);
#15809=ORIENTED_EDGE('',*,*,#10788,.F.);
#15810=ORIENTED_EDGE('',*,*,#10319,.F.);
#15811=ORIENTED_EDGE('',*,*,#10854,.T.);
#15812=ORIENTED_EDGE('',*,*,#10451,.T.);
#15813=ORIENTED_EDGE('',*,*,#10855,.F.);
#15814=ORIENTED_EDGE('',*,*,#10315,.F.);
#15815=ORIENTED_EDGE('',*,*,#10785,.T.);
#15816=ORIENTED_EDGE('',*,*,#10450,.T.);
#15817=ORIENTED_EDGE('',*,*,#10786,.F.);
#15818=ORIENTED_EDGE('',*,*,#10316,.F.);
#15819=ORIENTED_EDGE('',*,*,#10855,.T.);
#15820=ORIENTED_EDGE('',*,*,#10454,.T.);
#15821=ORIENTED_EDGE('',*,*,#10856,.F.);
#15822=ORIENTED_EDGE('',*,*,#10312,.F.);
#15823=ORIENTED_EDGE('',*,*,#10783,.T.);
#15824=ORIENTED_EDGE('',*,*,#10453,.T.);
#15825=ORIENTED_EDGE('',*,*,#10784,.F.);
#15826=ORIENTED_EDGE('',*,*,#10313,.F.);
#15827=ORIENTED_EDGE('',*,*,#10856,.T.);
#15828=ORIENTED_EDGE('',*,*,#10457,.T.);
#15829=ORIENTED_EDGE('',*,*,#10857,.F.);
#15830=ORIENTED_EDGE('',*,*,#10309,.F.);
#15831=ORIENTED_EDGE('',*,*,#10781,.T.);
#15832=ORIENTED_EDGE('',*,*,#10456,.T.);
#15833=ORIENTED_EDGE('',*,*,#10782,.F.);
#15834=ORIENTED_EDGE('',*,*,#10310,.F.);
#15835=ORIENTED_EDGE('',*,*,#10857,.T.);
#15836=ORIENTED_EDGE('',*,*,#10460,.T.);
#15837=ORIENTED_EDGE('',*,*,#10858,.F.);
#15838=ORIENTED_EDGE('',*,*,#10306,.F.);
#15839=ORIENTED_EDGE('',*,*,#10779,.T.);
#15840=ORIENTED_EDGE('',*,*,#10459,.T.);
#15841=ORIENTED_EDGE('',*,*,#10780,.F.);
#15842=ORIENTED_EDGE('',*,*,#10307,.F.);
#15843=ORIENTED_EDGE('',*,*,#10858,.T.);
#15844=ORIENTED_EDGE('',*,*,#10463,.T.);
#15845=ORIENTED_EDGE('',*,*,#10859,.F.);
#15846=ORIENTED_EDGE('',*,*,#10303,.F.);
#15847=ORIENTED_EDGE('',*,*,#10777,.T.);
#15848=ORIENTED_EDGE('',*,*,#10462,.T.);
#15849=ORIENTED_EDGE('',*,*,#10778,.F.);
#15850=ORIENTED_EDGE('',*,*,#10304,.F.);
#15851=ORIENTED_EDGE('',*,*,#10859,.T.);
#15852=ORIENTED_EDGE('',*,*,#10466,.T.);
#15853=ORIENTED_EDGE('',*,*,#10860,.F.);
#15854=ORIENTED_EDGE('',*,*,#10300,.F.);
#15855=ORIENTED_EDGE('',*,*,#10775,.T.);
#15856=ORIENTED_EDGE('',*,*,#10465,.T.);
#15857=ORIENTED_EDGE('',*,*,#10776,.F.);
#15858=ORIENTED_EDGE('',*,*,#10301,.F.);
#15859=ORIENTED_EDGE('',*,*,#10860,.T.);
#15860=ORIENTED_EDGE('',*,*,#10469,.T.);
#15861=ORIENTED_EDGE('',*,*,#10861,.F.);
#15862=ORIENTED_EDGE('',*,*,#10297,.F.);
#15863=ORIENTED_EDGE('',*,*,#10773,.T.);
#15864=ORIENTED_EDGE('',*,*,#10468,.T.);
#15865=ORIENTED_EDGE('',*,*,#10774,.F.);
#15866=ORIENTED_EDGE('',*,*,#10298,.F.);
#15867=ORIENTED_EDGE('',*,*,#10861,.T.);
#15868=ORIENTED_EDGE('',*,*,#10472,.T.);
#15869=ORIENTED_EDGE('',*,*,#10862,.F.);
#15870=ORIENTED_EDGE('',*,*,#10294,.F.);
#15871=ORIENTED_EDGE('',*,*,#10771,.T.);
#15872=ORIENTED_EDGE('',*,*,#10471,.T.);
#15873=ORIENTED_EDGE('',*,*,#10772,.F.);
#15874=ORIENTED_EDGE('',*,*,#10295,.F.);
#15875=ORIENTED_EDGE('',*,*,#10862,.T.);
#15876=ORIENTED_EDGE('',*,*,#10475,.T.);
#15877=ORIENTED_EDGE('',*,*,#10863,.F.);
#15878=ORIENTED_EDGE('',*,*,#10291,.F.);
#15879=ORIENTED_EDGE('',*,*,#10769,.T.);
#15880=ORIENTED_EDGE('',*,*,#10474,.T.);
#15881=ORIENTED_EDGE('',*,*,#10770,.F.);
#15882=ORIENTED_EDGE('',*,*,#10292,.F.);
#15883=ORIENTED_EDGE('',*,*,#10863,.T.);
#15884=ORIENTED_EDGE('',*,*,#10478,.T.);
#15885=ORIENTED_EDGE('',*,*,#10864,.F.);
#15886=ORIENTED_EDGE('',*,*,#10288,.F.);
#15887=ORIENTED_EDGE('',*,*,#10767,.T.);
#15888=ORIENTED_EDGE('',*,*,#10477,.T.);
#15889=ORIENTED_EDGE('',*,*,#10768,.F.);
#15890=ORIENTED_EDGE('',*,*,#10289,.F.);
#15891=ORIENTED_EDGE('',*,*,#10864,.T.);
#15892=ORIENTED_EDGE('',*,*,#10481,.T.);
#15893=ORIENTED_EDGE('',*,*,#10865,.F.);
#15894=ORIENTED_EDGE('',*,*,#10285,.F.);
#15895=ORIENTED_EDGE('',*,*,#10765,.T.);
#15896=ORIENTED_EDGE('',*,*,#10480,.T.);
#15897=ORIENTED_EDGE('',*,*,#10766,.F.);
#15898=ORIENTED_EDGE('',*,*,#10286,.F.);
#15899=ORIENTED_EDGE('',*,*,#10865,.T.);
#15900=ORIENTED_EDGE('',*,*,#10484,.T.);
#15901=ORIENTED_EDGE('',*,*,#10866,.F.);
#15902=ORIENTED_EDGE('',*,*,#10282,.F.);
#15903=ORIENTED_EDGE('',*,*,#10763,.T.);
#15904=ORIENTED_EDGE('',*,*,#10483,.T.);
#15905=ORIENTED_EDGE('',*,*,#10764,.F.);
#15906=ORIENTED_EDGE('',*,*,#10283,.F.);
#15907=ORIENTED_EDGE('',*,*,#10866,.T.);
#15908=ORIENTED_EDGE('',*,*,#10487,.T.);
#15909=ORIENTED_EDGE('',*,*,#10867,.F.);
#15910=ORIENTED_EDGE('',*,*,#10279,.F.);
#15911=ORIENTED_EDGE('',*,*,#10761,.T.);
#15912=ORIENTED_EDGE('',*,*,#10486,.T.);
#15913=ORIENTED_EDGE('',*,*,#10762,.F.);
#15914=ORIENTED_EDGE('',*,*,#10280,.F.);
#15915=ORIENTED_EDGE('',*,*,#10867,.T.);
#15916=ORIENTED_EDGE('',*,*,#10490,.T.);
#15917=ORIENTED_EDGE('',*,*,#10868,.F.);
#15918=ORIENTED_EDGE('',*,*,#10276,.F.);
#15919=ORIENTED_EDGE('',*,*,#10759,.T.);
#15920=ORIENTED_EDGE('',*,*,#10489,.T.);
#15921=ORIENTED_EDGE('',*,*,#10760,.F.);
#15922=ORIENTED_EDGE('',*,*,#10277,.F.);
#15923=ORIENTED_EDGE('',*,*,#10868,.T.);
#15924=ORIENTED_EDGE('',*,*,#10493,.T.);
#15925=ORIENTED_EDGE('',*,*,#10869,.F.);
#15926=ORIENTED_EDGE('',*,*,#10273,.F.);
#15927=ORIENTED_EDGE('',*,*,#10757,.T.);
#15928=ORIENTED_EDGE('',*,*,#10492,.T.);
#15929=ORIENTED_EDGE('',*,*,#10758,.F.);
#15930=ORIENTED_EDGE('',*,*,#10274,.F.);
#15931=ORIENTED_EDGE('',*,*,#10869,.T.);
#15932=ORIENTED_EDGE('',*,*,#10496,.T.);
#15933=ORIENTED_EDGE('',*,*,#10870,.F.);
#15934=ORIENTED_EDGE('',*,*,#10270,.F.);
#15935=ORIENTED_EDGE('',*,*,#10755,.T.);
#15936=ORIENTED_EDGE('',*,*,#10495,.T.);
#15937=ORIENTED_EDGE('',*,*,#10756,.F.);
#15938=ORIENTED_EDGE('',*,*,#10271,.F.);
#15939=ORIENTED_EDGE('',*,*,#10870,.T.);
#15940=ORIENTED_EDGE('',*,*,#10499,.T.);
#15941=ORIENTED_EDGE('',*,*,#10871,.F.);
#15942=ORIENTED_EDGE('',*,*,#10267,.F.);
#15943=ORIENTED_EDGE('',*,*,#10753,.T.);
#15944=ORIENTED_EDGE('',*,*,#10498,.T.);
#15945=ORIENTED_EDGE('',*,*,#10754,.F.);
#15946=ORIENTED_EDGE('',*,*,#10268,.F.);
#15947=ORIENTED_EDGE('',*,*,#10871,.T.);
#15948=ORIENTED_EDGE('',*,*,#10502,.T.);
#15949=ORIENTED_EDGE('',*,*,#10872,.F.);
#15950=ORIENTED_EDGE('',*,*,#10264,.F.);
#15951=ORIENTED_EDGE('',*,*,#10751,.T.);
#15952=ORIENTED_EDGE('',*,*,#10501,.T.);
#15953=ORIENTED_EDGE('',*,*,#10752,.F.);
#15954=ORIENTED_EDGE('',*,*,#10265,.F.);
#15955=ORIENTED_EDGE('',*,*,#10872,.T.);
#15956=ORIENTED_EDGE('',*,*,#10505,.T.);
#15957=ORIENTED_EDGE('',*,*,#10873,.F.);
#15958=ORIENTED_EDGE('',*,*,#10261,.F.);
#15959=ORIENTED_EDGE('',*,*,#10749,.T.);
#15960=ORIENTED_EDGE('',*,*,#10504,.T.);
#15961=ORIENTED_EDGE('',*,*,#10750,.F.);
#15962=ORIENTED_EDGE('',*,*,#10262,.F.);
#15963=ORIENTED_EDGE('',*,*,#10873,.T.);
#15964=ORIENTED_EDGE('',*,*,#10508,.T.);
#15965=ORIENTED_EDGE('',*,*,#10874,.F.);
#15966=ORIENTED_EDGE('',*,*,#10258,.F.);
#15967=ORIENTED_EDGE('',*,*,#10747,.T.);
#15968=ORIENTED_EDGE('',*,*,#10507,.T.);
#15969=ORIENTED_EDGE('',*,*,#10748,.F.);
#15970=ORIENTED_EDGE('',*,*,#10259,.F.);
#15971=ORIENTED_EDGE('',*,*,#10874,.T.);
#15972=ORIENTED_EDGE('',*,*,#10511,.T.);
#15973=ORIENTED_EDGE('',*,*,#10875,.F.);
#15974=ORIENTED_EDGE('',*,*,#10255,.F.);
#15975=ORIENTED_EDGE('',*,*,#10745,.T.);
#15976=ORIENTED_EDGE('',*,*,#10510,.T.);
#15977=ORIENTED_EDGE('',*,*,#10746,.F.);
#15978=ORIENTED_EDGE('',*,*,#10256,.F.);
#15979=ORIENTED_EDGE('',*,*,#10875,.T.);
#15980=ORIENTED_EDGE('',*,*,#10514,.T.);
#15981=ORIENTED_EDGE('',*,*,#10876,.F.);
#15982=ORIENTED_EDGE('',*,*,#10252,.F.);
#15983=ORIENTED_EDGE('',*,*,#10743,.T.);
#15984=ORIENTED_EDGE('',*,*,#10513,.T.);
#15985=ORIENTED_EDGE('',*,*,#10744,.F.);
#15986=ORIENTED_EDGE('',*,*,#10253,.F.);
#15987=ORIENTED_EDGE('',*,*,#10876,.T.);
#15988=ORIENTED_EDGE('',*,*,#10517,.T.);
#15989=ORIENTED_EDGE('',*,*,#10877,.F.);
#15990=ORIENTED_EDGE('',*,*,#10249,.F.);
#15991=ORIENTED_EDGE('',*,*,#10741,.T.);
#15992=ORIENTED_EDGE('',*,*,#10516,.T.);
#15993=ORIENTED_EDGE('',*,*,#10742,.F.);
#15994=ORIENTED_EDGE('',*,*,#10250,.F.);
#15995=ORIENTED_EDGE('',*,*,#10877,.T.);
#15996=ORIENTED_EDGE('',*,*,#10520,.T.);
#15997=ORIENTED_EDGE('',*,*,#10878,.F.);
#15998=ORIENTED_EDGE('',*,*,#10246,.F.);
#15999=ORIENTED_EDGE('',*,*,#10739,.T.);
#16000=ORIENTED_EDGE('',*,*,#10519,.T.);
#16001=ORIENTED_EDGE('',*,*,#10740,.F.);
#16002=ORIENTED_EDGE('',*,*,#10247,.F.);
#16003=ORIENTED_EDGE('',*,*,#10878,.T.);
#16004=ORIENTED_EDGE('',*,*,#10523,.T.);
#16005=ORIENTED_EDGE('',*,*,#10879,.F.);
#16006=ORIENTED_EDGE('',*,*,#10243,.F.);
#16007=ORIENTED_EDGE('',*,*,#10737,.T.);
#16008=ORIENTED_EDGE('',*,*,#10522,.T.);
#16009=ORIENTED_EDGE('',*,*,#10738,.F.);
#16010=ORIENTED_EDGE('',*,*,#10244,.F.);
#16011=ORIENTED_EDGE('',*,*,#10879,.T.);
#16012=ORIENTED_EDGE('',*,*,#10526,.T.);
#16013=ORIENTED_EDGE('',*,*,#10880,.F.);
#16014=ORIENTED_EDGE('',*,*,#10240,.F.);
#16015=ORIENTED_EDGE('',*,*,#10735,.T.);
#16016=ORIENTED_EDGE('',*,*,#10525,.T.);
#16017=ORIENTED_EDGE('',*,*,#10736,.F.);
#16018=ORIENTED_EDGE('',*,*,#10241,.F.);
#16019=ORIENTED_EDGE('',*,*,#10880,.T.);
#16020=ORIENTED_EDGE('',*,*,#10529,.T.);
#16021=ORIENTED_EDGE('',*,*,#10881,.F.);
#16022=ORIENTED_EDGE('',*,*,#10237,.F.);
#16023=ORIENTED_EDGE('',*,*,#10733,.T.);
#16024=ORIENTED_EDGE('',*,*,#10528,.T.);
#16025=ORIENTED_EDGE('',*,*,#10734,.F.);
#16026=ORIENTED_EDGE('',*,*,#10238,.F.);
#16027=ORIENTED_EDGE('',*,*,#10881,.T.);
#16028=ORIENTED_EDGE('',*,*,#10532,.T.);
#16029=ORIENTED_EDGE('',*,*,#10882,.F.);
#16030=ORIENTED_EDGE('',*,*,#10234,.F.);
#16031=ORIENTED_EDGE('',*,*,#10731,.T.);
#16032=ORIENTED_EDGE('',*,*,#10531,.T.);
#16033=ORIENTED_EDGE('',*,*,#10732,.F.);
#16034=ORIENTED_EDGE('',*,*,#10235,.F.);
#16035=ORIENTED_EDGE('',*,*,#10882,.T.);
#16036=ORIENTED_EDGE('',*,*,#10535,.T.);
#16037=ORIENTED_EDGE('',*,*,#10883,.F.);
#16038=ORIENTED_EDGE('',*,*,#10231,.F.);
#16039=ORIENTED_EDGE('',*,*,#10729,.T.);
#16040=ORIENTED_EDGE('',*,*,#10534,.T.);
#16041=ORIENTED_EDGE('',*,*,#10730,.F.);
#16042=ORIENTED_EDGE('',*,*,#10232,.F.);
#16043=ORIENTED_EDGE('',*,*,#10883,.T.);
#16044=ORIENTED_EDGE('',*,*,#10538,.T.);
#16045=ORIENTED_EDGE('',*,*,#10884,.F.);
#16046=ORIENTED_EDGE('',*,*,#10228,.F.);
#16047=ORIENTED_EDGE('',*,*,#10727,.T.);
#16048=ORIENTED_EDGE('',*,*,#10537,.T.);
#16049=ORIENTED_EDGE('',*,*,#10728,.F.);
#16050=ORIENTED_EDGE('',*,*,#10229,.F.);
#16051=ORIENTED_EDGE('',*,*,#10884,.T.);
#16052=ORIENTED_EDGE('',*,*,#10541,.T.);
#16053=ORIENTED_EDGE('',*,*,#10885,.F.);
#16054=ORIENTED_EDGE('',*,*,#10225,.F.);
#16055=ORIENTED_EDGE('',*,*,#10725,.T.);
#16056=ORIENTED_EDGE('',*,*,#10540,.T.);
#16057=ORIENTED_EDGE('',*,*,#10726,.F.);
#16058=ORIENTED_EDGE('',*,*,#10226,.F.);
#16059=ORIENTED_EDGE('',*,*,#10885,.T.);
#16060=ORIENTED_EDGE('',*,*,#10544,.T.);
#16061=ORIENTED_EDGE('',*,*,#10886,.F.);
#16062=ORIENTED_EDGE('',*,*,#10222,.F.);
#16063=ORIENTED_EDGE('',*,*,#10723,.T.);
#16064=ORIENTED_EDGE('',*,*,#10543,.T.);
#16065=ORIENTED_EDGE('',*,*,#10724,.F.);
#16066=ORIENTED_EDGE('',*,*,#10223,.F.);
#16067=ORIENTED_EDGE('',*,*,#10886,.T.);
#16068=ORIENTED_EDGE('',*,*,#10547,.T.);
#16069=ORIENTED_EDGE('',*,*,#10887,.F.);
#16070=ORIENTED_EDGE('',*,*,#10219,.F.);
#16071=ORIENTED_EDGE('',*,*,#10721,.T.);
#16072=ORIENTED_EDGE('',*,*,#10546,.T.);
#16073=ORIENTED_EDGE('',*,*,#10722,.F.);
#16074=ORIENTED_EDGE('',*,*,#10220,.F.);
#16075=ORIENTED_EDGE('',*,*,#10887,.T.);
#16076=ORIENTED_EDGE('',*,*,#10550,.T.);
#16077=ORIENTED_EDGE('',*,*,#10888,.F.);
#16078=ORIENTED_EDGE('',*,*,#10216,.F.);
#16079=ORIENTED_EDGE('',*,*,#10719,.T.);
#16080=ORIENTED_EDGE('',*,*,#10549,.T.);
#16081=ORIENTED_EDGE('',*,*,#10720,.F.);
#16082=ORIENTED_EDGE('',*,*,#10217,.F.);
#16083=ORIENTED_EDGE('',*,*,#10888,.T.);
#16084=ORIENTED_EDGE('',*,*,#10553,.T.);
#16085=ORIENTED_EDGE('',*,*,#10889,.F.);
#16086=ORIENTED_EDGE('',*,*,#10213,.F.);
#16087=ORIENTED_EDGE('',*,*,#10717,.T.);
#16088=ORIENTED_EDGE('',*,*,#10552,.T.);
#16089=ORIENTED_EDGE('',*,*,#10718,.F.);
#16090=ORIENTED_EDGE('',*,*,#10214,.F.);
#16091=ORIENTED_EDGE('',*,*,#10889,.T.);
#16092=ORIENTED_EDGE('',*,*,#10556,.T.);
#16093=ORIENTED_EDGE('',*,*,#10890,.F.);
#16094=ORIENTED_EDGE('',*,*,#10210,.F.);
#16095=ORIENTED_EDGE('',*,*,#10715,.T.);
#16096=ORIENTED_EDGE('',*,*,#10555,.T.);
#16097=ORIENTED_EDGE('',*,*,#10716,.F.);
#16098=ORIENTED_EDGE('',*,*,#10211,.F.);
#16099=ORIENTED_EDGE('',*,*,#10890,.T.);
#16100=ORIENTED_EDGE('',*,*,#10562,.T.);
#16101=ORIENTED_EDGE('',*,*,#10891,.F.);
#16102=ORIENTED_EDGE('',*,*,#10441,.F.);
#16103=ORIENTED_EDGE('',*,*,#10713,.T.);
#16104=ORIENTED_EDGE('',*,*,#10561,.T.);
#16105=ORIENTED_EDGE('',*,*,#10558,.T.);
#16106=ORIENTED_EDGE('',*,*,#10714,.F.);
#16107=ORIENTED_EDGE('',*,*,#10208,.F.);
#16108=ORIENTED_EDGE('',*,*,#10891,.T.);
#16109=ORIENTED_EDGE('',*,*,#10565,.T.);
#16110=ORIENTED_EDGE('',*,*,#10892,.F.);
#16111=ORIENTED_EDGE('',*,*,#10438,.F.);
#16112=ORIENTED_EDGE('',*,*,#10711,.T.);
#16113=ORIENTED_EDGE('',*,*,#10564,.T.);
#16114=ORIENTED_EDGE('',*,*,#10712,.F.);
#16115=ORIENTED_EDGE('',*,*,#10439,.F.);
#16116=ORIENTED_EDGE('',*,*,#10892,.T.);
#16117=ORIENTED_EDGE('',*,*,#10568,.T.);
#16118=ORIENTED_EDGE('',*,*,#10893,.F.);
#16119=ORIENTED_EDGE('',*,*,#10435,.F.);
#16120=ORIENTED_EDGE('',*,*,#10709,.T.);
#16121=ORIENTED_EDGE('',*,*,#10567,.T.);
#16122=ORIENTED_EDGE('',*,*,#10710,.F.);
#16123=ORIENTED_EDGE('',*,*,#10436,.F.);
#16124=ORIENTED_EDGE('',*,*,#10893,.T.);
#16125=ORIENTED_EDGE('',*,*,#10571,.T.);
#16126=ORIENTED_EDGE('',*,*,#10894,.F.);
#16127=ORIENTED_EDGE('',*,*,#10432,.F.);
#16128=ORIENTED_EDGE('',*,*,#10707,.T.);
#16129=ORIENTED_EDGE('',*,*,#10570,.T.);
#16130=ORIENTED_EDGE('',*,*,#10708,.F.);
#16131=ORIENTED_EDGE('',*,*,#10433,.F.);
#16132=ORIENTED_EDGE('',*,*,#10894,.T.);
#16133=ORIENTED_EDGE('',*,*,#10574,.T.);
#16134=ORIENTED_EDGE('',*,*,#10895,.F.);
#16135=ORIENTED_EDGE('',*,*,#10429,.F.);
#16136=ORIENTED_EDGE('',*,*,#10705,.T.);
#16137=ORIENTED_EDGE('',*,*,#10573,.T.);
#16138=ORIENTED_EDGE('',*,*,#10706,.F.);
#16139=ORIENTED_EDGE('',*,*,#10430,.F.);
#16140=ORIENTED_EDGE('',*,*,#10895,.T.);
#16141=ORIENTED_EDGE('',*,*,#10577,.T.);
#16142=ORIENTED_EDGE('',*,*,#10896,.F.);
#16143=ORIENTED_EDGE('',*,*,#10426,.F.);
#16144=ORIENTED_EDGE('',*,*,#10703,.T.);
#16145=ORIENTED_EDGE('',*,*,#10576,.T.);
#16146=ORIENTED_EDGE('',*,*,#10704,.F.);
#16147=ORIENTED_EDGE('',*,*,#10427,.F.);
#16148=ORIENTED_EDGE('',*,*,#10896,.T.);
#16149=ORIENTED_EDGE('',*,*,#10580,.T.);
#16150=ORIENTED_EDGE('',*,*,#10897,.F.);
#16151=ORIENTED_EDGE('',*,*,#10423,.F.);
#16152=ORIENTED_EDGE('',*,*,#10701,.T.);
#16153=ORIENTED_EDGE('',*,*,#10579,.T.);
#16154=ORIENTED_EDGE('',*,*,#10702,.F.);
#16155=ORIENTED_EDGE('',*,*,#10424,.F.);
#16156=ORIENTED_EDGE('',*,*,#10897,.T.);
#16157=ORIENTED_EDGE('',*,*,#10583,.T.);
#16158=ORIENTED_EDGE('',*,*,#10898,.F.);
#16159=ORIENTED_EDGE('',*,*,#10420,.F.);
#16160=ORIENTED_EDGE('',*,*,#10699,.T.);
#16161=ORIENTED_EDGE('',*,*,#10582,.T.);
#16162=ORIENTED_EDGE('',*,*,#10700,.F.);
#16163=ORIENTED_EDGE('',*,*,#10421,.F.);
#16164=ORIENTED_EDGE('',*,*,#10898,.T.);
#16165=ORIENTED_EDGE('',*,*,#10586,.T.);
#16166=ORIENTED_EDGE('',*,*,#10899,.F.);
#16167=ORIENTED_EDGE('',*,*,#10417,.F.);
#16168=ORIENTED_EDGE('',*,*,#10697,.T.);
#16169=ORIENTED_EDGE('',*,*,#10585,.T.);
#16170=ORIENTED_EDGE('',*,*,#10698,.F.);
#16171=ORIENTED_EDGE('',*,*,#10418,.F.);
#16172=ORIENTED_EDGE('',*,*,#10899,.T.);
#16173=ORIENTED_EDGE('',*,*,#10589,.T.);
#16174=ORIENTED_EDGE('',*,*,#10900,.F.);
#16175=ORIENTED_EDGE('',*,*,#10414,.F.);
#16176=ORIENTED_EDGE('',*,*,#10695,.T.);
#16177=ORIENTED_EDGE('',*,*,#10588,.T.);
#16178=ORIENTED_EDGE('',*,*,#10696,.F.);
#16179=ORIENTED_EDGE('',*,*,#10415,.F.);
#16180=ORIENTED_EDGE('',*,*,#10900,.T.);
#16181=ORIENTED_EDGE('',*,*,#10592,.T.);
#16182=ORIENTED_EDGE('',*,*,#10901,.F.);
#16183=ORIENTED_EDGE('',*,*,#10411,.F.);
#16184=ORIENTED_EDGE('',*,*,#10693,.T.);
#16185=ORIENTED_EDGE('',*,*,#10591,.T.);
#16186=ORIENTED_EDGE('',*,*,#10694,.F.);
#16187=ORIENTED_EDGE('',*,*,#10412,.F.);
#16188=ORIENTED_EDGE('',*,*,#10901,.T.);
#16189=ORIENTED_EDGE('',*,*,#10595,.T.);
#16190=ORIENTED_EDGE('',*,*,#10902,.F.);
#16191=ORIENTED_EDGE('',*,*,#10408,.F.);
#16192=ORIENTED_EDGE('',*,*,#10691,.T.);
#16193=ORIENTED_EDGE('',*,*,#10594,.T.);
#16194=ORIENTED_EDGE('',*,*,#10692,.F.);
#16195=ORIENTED_EDGE('',*,*,#10409,.F.);
#16196=ORIENTED_EDGE('',*,*,#10902,.T.);
#16197=ORIENTED_EDGE('',*,*,#10598,.T.);
#16198=ORIENTED_EDGE('',*,*,#10903,.F.);
#16199=ORIENTED_EDGE('',*,*,#10405,.F.);
#16200=ORIENTED_EDGE('',*,*,#10689,.T.);
#16201=ORIENTED_EDGE('',*,*,#10597,.T.);
#16202=ORIENTED_EDGE('',*,*,#10690,.F.);
#16203=ORIENTED_EDGE('',*,*,#10406,.F.);
#16204=ORIENTED_EDGE('',*,*,#10903,.T.);
#16205=ORIENTED_EDGE('',*,*,#10601,.T.);
#16206=ORIENTED_EDGE('',*,*,#10904,.F.);
#16207=ORIENTED_EDGE('',*,*,#10402,.F.);
#16208=ORIENTED_EDGE('',*,*,#10687,.T.);
#16209=ORIENTED_EDGE('',*,*,#10600,.T.);
#16210=ORIENTED_EDGE('',*,*,#10688,.F.);
#16211=ORIENTED_EDGE('',*,*,#10403,.F.);
#16212=ORIENTED_EDGE('',*,*,#10904,.T.);
#16213=ORIENTED_EDGE('',*,*,#10604,.T.);
#16214=ORIENTED_EDGE('',*,*,#10905,.F.);
#16215=ORIENTED_EDGE('',*,*,#10399,.F.);
#16216=ORIENTED_EDGE('',*,*,#10685,.T.);
#16217=ORIENTED_EDGE('',*,*,#10603,.T.);
#16218=ORIENTED_EDGE('',*,*,#10686,.F.);
#16219=ORIENTED_EDGE('',*,*,#10400,.F.);
#16220=ORIENTED_EDGE('',*,*,#10905,.T.);
#16221=ORIENTED_EDGE('',*,*,#10607,.T.);
#16222=ORIENTED_EDGE('',*,*,#10906,.F.);
#16223=ORIENTED_EDGE('',*,*,#10396,.F.);
#16224=ORIENTED_EDGE('',*,*,#10683,.T.);
#16225=ORIENTED_EDGE('',*,*,#10606,.T.);
#16226=ORIENTED_EDGE('',*,*,#10684,.F.);
#16227=ORIENTED_EDGE('',*,*,#10397,.F.);
#16228=ORIENTED_EDGE('',*,*,#10906,.T.);
#16229=ORIENTED_EDGE('',*,*,#10610,.T.);
#16230=ORIENTED_EDGE('',*,*,#10907,.F.);
#16231=ORIENTED_EDGE('',*,*,#10393,.F.);
#16232=ORIENTED_EDGE('',*,*,#10681,.T.);
#16233=ORIENTED_EDGE('',*,*,#10609,.T.);
#16234=ORIENTED_EDGE('',*,*,#10682,.F.);
#16235=ORIENTED_EDGE('',*,*,#10394,.F.);
#16236=ORIENTED_EDGE('',*,*,#10907,.T.);
#16237=ORIENTED_EDGE('',*,*,#10613,.T.);
#16238=ORIENTED_EDGE('',*,*,#10908,.F.);
#16239=ORIENTED_EDGE('',*,*,#10390,.F.);
#16240=ORIENTED_EDGE('',*,*,#10678,.T.);
#16241=ORIENTED_EDGE('',*,*,#10612,.T.);
#16242=ORIENTED_EDGE('',*,*,#10680,.F.);
#16243=ORIENTED_EDGE('',*,*,#10391,.F.);
#16244=ORIENTED_EDGE('',*,*,#10908,.T.);
#16245=CYLINDRICAL_SURFACE('',#17789,22.5);
#16246=CYLINDRICAL_SURFACE('',#17792,25.);
#16247=CYLINDRICAL_SURFACE('',#17802,10.5);
#16248=CYLINDRICAL_SURFACE('',#17806,22.5);
#16249=CYLINDRICAL_SURFACE('',#17807,22.5);
#16250=CYLINDRICAL_SURFACE('',#17810,10.5);
#16251=CYLINDRICAL_SURFACE('',#17813,25.);
#16252=CYLINDRICAL_SURFACE('',#17823,22.5);
#16253=CYLINDRICAL_SURFACE('',#17834,10.5);
#16254=CYLINDRICAL_SURFACE('',#17837,22.5);
#16255=CYLINDRICAL_SURFACE('',#17840,22.5);
#16256=CYLINDRICAL_SURFACE('',#17850,10.5);
#16257=CYLINDRICAL_SURFACE('',#17853,22.5);
#16258=CYLINDRICAL_SURFACE('',#17856,22.5);
#16259=CYLINDRICAL_SURFACE('',#17858,10.);
#16260=CYLINDRICAL_SURFACE('',#17867,8.);
#16261=CYLINDRICAL_SURFACE('',#17868,8.);
#16262=CYLINDRICAL_SURFACE('',#17871,10.);
#16263=CYLINDRICAL_SURFACE('',#17886,8.);
#16264=CYLINDRICAL_SURFACE('',#17891,8.);
#16265=CYLINDRICAL_SURFACE('',#17894,2.6);
#16266=CYLINDRICAL_SURFACE('',#17902,8.);
#16267=CYLINDRICAL_SURFACE('',#17910,4.29685191531258);
#16268=CYLINDRICAL_SURFACE('',#17911,4.29685191531258);
#16269=CYLINDRICAL_SURFACE('',#17912,4.29685191531258);
#16270=CYLINDRICAL_SURFACE('',#17913,4.29685191531258);
#16271=CYLINDRICAL_SURFACE('',#17914,4.29685191531258);
#16272=CYLINDRICAL_SURFACE('',#17915,4.29685191531258);
#16273=CYLINDRICAL_SURFACE('',#17916,4.29685191531258);
#16274=CYLINDRICAL_SURFACE('',#17917,4.29685191531258);
#16275=CYLINDRICAL_SURFACE('',#17918,4.29685191531258);
#16276=CYLINDRICAL_SURFACE('',#17919,4.29685191531258);
#16277=CYLINDRICAL_SURFACE('',#17920,4.29685191531258);
#16278=CYLINDRICAL_SURFACE('',#17921,4.29685191531258);
#16279=CYLINDRICAL_SURFACE('',#17922,4.29685191531258);
#16280=CYLINDRICAL_SURFACE('',#17923,4.29685191531258);
#16281=CYLINDRICAL_SURFACE('',#17924,4.29685191531258);
#16282=CYLINDRICAL_SURFACE('',#17925,4.29685191531258);
#16283=CYLINDRICAL_SURFACE('',#17926,4.29685191531258);
#16284=CYLINDRICAL_SURFACE('',#17927,4.29685191531258);
#16285=CYLINDRICAL_SURFACE('',#17928,4.29685191531258);
#16286=CYLINDRICAL_SURFACE('',#17929,4.29685191531258);
#16287=CYLINDRICAL_SURFACE('',#17930,4.29685191531258);
#16288=CYLINDRICAL_SURFACE('',#17931,4.29685191531258);
#16289=CYLINDRICAL_SURFACE('',#17932,4.29685191531258);
#16290=CYLINDRICAL_SURFACE('',#17933,4.29685191531258);
#16291=CYLINDRICAL_SURFACE('',#17934,4.29685191531258);
#16292=CYLINDRICAL_SURFACE('',#17936,4.12499999999999);
#16293=CYLINDRICAL_SURFACE('',#17938,4.12499999999999);
#16294=CYLINDRICAL_SURFACE('',#17940,4.12499999999999);
#16295=CYLINDRICAL_SURFACE('',#17941,4.12499999999999);
#16296=CYLINDRICAL_SURFACE('',#17942,4.12499999999999);
#16297=CYLINDRICAL_SURFACE('',#17943,4.12499999999999);
#16298=CYLINDRICAL_SURFACE('',#17944,4.12499999999999);
#16299=CYLINDRICAL_SURFACE('',#17945,4.12499999999999);
#16300=CYLINDRICAL_SURFACE('',#17946,4.12499999999999);
#16301=CYLINDRICAL_SURFACE('',#17947,4.12499999999999);
#16302=CYLINDRICAL_SURFACE('',#17948,4.12499999999999);
#16303=CYLINDRICAL_SURFACE('',#17949,4.12499999999999);
#16304=CYLINDRICAL_SURFACE('',#17950,4.12499999999999);
#16305=CYLINDRICAL_SURFACE('',#17951,4.12499999999999);
#16306=CYLINDRICAL_SURFACE('',#17952,4.12499999999999);
#16307=CYLINDRICAL_SURFACE('',#17953,4.12499999999999);
#16308=CYLINDRICAL_SURFACE('',#17954,4.12499999999999);
#16309=CYLINDRICAL_SURFACE('',#17955,4.12499999999999);
#16310=CYLINDRICAL_SURFACE('',#17956,4.12499999999999);
#16311=CYLINDRICAL_SURFACE('',#17957,4.12499999999999);
#16312=CYLINDRICAL_SURFACE('',#17958,4.12499999999999);
#16313=CYLINDRICAL_SURFACE('',#17959,4.12499999999999);
#16314=CYLINDRICAL_SURFACE('',#17960,4.12499999999999);
#16315=CYLINDRICAL_SURFACE('',#17961,4.12499999999999);
#16316=CYLINDRICAL_SURFACE('',#17962,4.12499999999999);
#16317=CYLINDRICAL_SURFACE('',#17966,8.);
#16318=CYLINDRICAL_SURFACE('',#17977,12.5);
#16319=CYLINDRICAL_SURFACE('',#17987,25.);
#16320=CYLINDRICAL_SURFACE('',#17989,22.5);
#16321=CYLINDRICAL_SURFACE('',#17992,4.12499999999999);
#16322=CYLINDRICAL_SURFACE('',#18001,4.29685191531258);
#16323=CYLINDRICAL_SURFACE('',#18003,8.05);
#16324=CYLINDRICAL_SURFACE('',#18006,10.5);
#16325=CYLINDRICAL_SURFACE('',#18013,22.5);
#16326=CYLINDRICAL_SURFACE('',#18016,25.);
#16327=CYLINDRICAL_SURFACE('',#18031,2.5);
#16328=CYLINDRICAL_SURFACE('',#18033,3.);
#16329=CYLINDRICAL_SURFACE('',#18041,10.);
#16330=CYLINDRICAL_SURFACE('',#18045,4.);
#16331=CYLINDRICAL_SURFACE('',#18053,5.);
#16332=CYLINDRICAL_SURFACE('',#18070,6.);
#16333=CYLINDRICAL_SURFACE('',#18086,6.);
#16334=CYLINDRICAL_SURFACE('',#18093,9.25);
#16335=CYLINDRICAL_SURFACE('',#18094,1.);
#16336=CYLINDRICAL_SURFACE('',#18097,1.);
#16337=CYLINDRICAL_SURFACE('',#18109,1.);
#16338=CYLINDRICAL_SURFACE('',#18121,1.);
#16339=CYLINDRICAL_SURFACE('',#18133,6.);
#16340=CYLINDRICAL_SURFACE('',#18142,6.);
#16341=CYLINDRICAL_SURFACE('',#18154,5.5);
#16342=CYLINDRICAL_SURFACE('',#18170,4.);
#16343=CYLINDRICAL_SURFACE('',#18202,6.);
#16344=CYLINDRICAL_SURFACE('',#18211,4.);
#16345=CYLINDRICAL_SURFACE('',#18227,5.);
#16346=CYLINDRICAL_SURFACE('',#18233,4.25);
#16347=CYLINDRICAL_SURFACE('',#18235,6.);
#16348=CYLINDRICAL_SURFACE('',#18238,12.5);
#16349=CYLINDRICAL_SURFACE('',#18250,2.);
#16350=CYLINDRICAL_SURFACE('',#18263,2.);
#16351=CYLINDRICAL_SURFACE('',#18271,2.);
#16352=CYLINDRICAL_SURFACE('',#18284,2.);
#16353=CYLINDRICAL_SURFACE('',#18287,6.00000000000143);
#16354=CYLINDRICAL_SURFACE('',#18289,6.00000000000152);
#16355=CYLINDRICAL_SURFACE('',#18291,6.00000000000095);
#16356=CYLINDRICAL_SURFACE('',#18293,5.);
#16357=CYLINDRICAL_SURFACE('',#18296,12.5);
#16358=CYLINDRICAL_SURFACE('',#18299,25.);
#16359=CYLINDRICAL_SURFACE('',#18302,25.);
#16360=CYLINDRICAL_SURFACE('',#18305,25.);
#16361=CYLINDRICAL_SURFACE('',#18308,25.);
#16362=CYLINDRICAL_SURFACE('',#18311,25.);
#16363=CYLINDRICAL_SURFACE('',#18361,25.);
#16364=CYLINDRICAL_SURFACE('',#18375,6.00000000000022);
#16365=CYLINDRICAL_SURFACE('',#18377,6.00000000000081);
#16366=CYLINDRICAL_SURFACE('',#18379,6.);
#16367=CYLINDRICAL_SURFACE('',#18390,2.);
#16368=CYLINDRICAL_SURFACE('',#18391,2.);
#16369=CYLINDRICAL_SURFACE('',#18401,2.);
#16370=CYLINDRICAL_SURFACE('',#18418,2.);
#16371=CYLINDRICAL_SURFACE('',#18420,2.);
#16372=CYLINDRICAL_SURFACE('',#18427,2.);
#16373=CYLINDRICAL_SURFACE('',#18438,2.);
#16374=CYLINDRICAL_SURFACE('',#18440,2.);
#16375=CYLINDRICAL_SURFACE('',#18482,2.);
#16376=CYLINDRICAL_SURFACE('',#18485,2.);
#16377=CYLINDRICAL_SURFACE('',#18487,1.2);
#16378=CYLINDRICAL_SURFACE('',#18488,3.2);
#16379=CYLINDRICAL_SURFACE('',#18489,2.);
#16380=CYLINDRICAL_SURFACE('',#18490,1.5);
#16381=CYLINDRICAL_SURFACE('',#18506,4.);
#16382=CYLINDRICAL_SURFACE('',#18511,4.);
#16383=CYLINDRICAL_SURFACE('',#18525,3.);
#16384=CYLINDRICAL_SURFACE('',#18530,3.);
#16385=CYLINDRICAL_SURFACE('',#18532,0.300000000000002);
#16386=CYLINDRICAL_SURFACE('',#18535,0.3);
#16387=CYLINDRICAL_SURFACE('',#18537,0.300000000000002);
#16388=CYLINDRICAL_SURFACE('',#18540,0.300000000000002);
#16389=CYLINDRICAL_SURFACE('',#18542,0.300000000000002);
#16390=CYLINDRICAL_SURFACE('',#18550,0.3);
#16391=CYLINDRICAL_SURFACE('',#18552,0.300000000000002);
#16392=CYLINDRICAL_SURFACE('',#18555,0.300000000000002);
#16393=CYLINDRICAL_SURFACE('',#18557,0.300000000000002);
#16394=CYLINDRICAL_SURFACE('',#18559,0.300000000000002);
#16395=CYLINDRICAL_SURFACE('',#18561,0.300000000000002);
#16396=CYLINDRICAL_SURFACE('',#18569,0.300000000000002);
#16397=CYLINDRICAL_SURFACE('',#18571,0.300000000000002);
#16398=CYLINDRICAL_SURFACE('',#18573,0.300000000000002);
#16399=CYLINDRICAL_SURFACE('',#18575,0.300000000000002);
#16400=CYLINDRICAL_SURFACE('',#18579,0.300000000000002);
#16401=CYLINDRICAL_SURFACE('',#18582,0.300000000000002);
#16402=CYLINDRICAL_SURFACE('',#18584,0.300000000000002);
#16403=CYLINDRICAL_SURFACE('',#18586,0.300000000000002);
#16404=CYLINDRICAL_SURFACE('',#18588,0.300000000000002);
#16405=CYLINDRICAL_SURFACE('',#18590,0.300000000000002);
#16406=CYLINDRICAL_SURFACE('',#18607,1.2);
#16407=CYLINDRICAL_SURFACE('',#18610,2.5);
#16408=CYLINDRICAL_SURFACE('',#18613,3.);
#16409=CYLINDRICAL_SURFACE('',#18618,4.25);
#16410=CYLINDRICAL_SURFACE('',#18621,1.2);
#16411=CYLINDRICAL_SURFACE('',#18624,1.2);
#16412=CYLINDRICAL_SURFACE('',#18627,2.);
#16413=CYLINDRICAL_SURFACE('',#18631,1.5);
#16414=CYLINDRICAL_SURFACE('',#18640,1.5);
#16415=CYLINDRICAL_SURFACE('',#18650,2.5);
#16416=CYLINDRICAL_SURFACE('',#18670,2.);
#16417=CYLINDRICAL_SURFACE('',#18679,2.);
#16418=CYLINDRICAL_SURFACE('',#18688,2.);
#16419=CYLINDRICAL_SURFACE('',#18697,2.);
#16420=CYLINDRICAL_SURFACE('',#18706,2.);
#16421=CYLINDRICAL_SURFACE('',#18715,2.);
#16422=CYLINDRICAL_SURFACE('',#18724,2.);
#16423=CYLINDRICAL_SURFACE('',#18733,2.);
#16424=CYLINDRICAL_SURFACE('',#18742,2.);
#16425=CYLINDRICAL_SURFACE('',#18751,2.);
#16426=CYLINDRICAL_SURFACE('',#18760,2.);
#16427=CYLINDRICAL_SURFACE('',#18769,2.);
#16428=CYLINDRICAL_SURFACE('',#18778,2.);
#16429=CYLINDRICAL_SURFACE('',#18787,2.);
#16430=CYLINDRICAL_SURFACE('',#18954,2.);
#16431=CYLINDRICAL_SURFACE('',#18955,8.175);
#16432=CYLINDRICAL_SURFACE('',#18956,8.175);
#16433=CYLINDRICAL_SURFACE('',#18957,8.175);
#16434=CYLINDRICAL_SURFACE('',#18958,8.175);
#16435=CYLINDRICAL_SURFACE('',#18959,8.175);
#16436=CYLINDRICAL_SURFACE('',#18960,8.175);
#16437=CYLINDRICAL_SURFACE('',#18961,8.175);
#16438=CYLINDRICAL_SURFACE('',#18962,8.175);
#16439=CYLINDRICAL_SURFACE('',#18963,8.175);
#16440=CYLINDRICAL_SURFACE('',#18964,8.175);
#16441=CYLINDRICAL_SURFACE('',#18965,8.175);
#16442=CYLINDRICAL_SURFACE('',#18966,8.175);
#16443=CYLINDRICAL_SURFACE('',#18967,8.175);
#16444=CYLINDRICAL_SURFACE('',#18968,8.175);
#16445=CYLINDRICAL_SURFACE('',#18969,8.175);
#16446=CYLINDRICAL_SURFACE('',#18970,8.175);
#16447=CYLINDRICAL_SURFACE('',#18971,8.175);
#16448=CYLINDRICAL_SURFACE('',#18972,8.175);
#16449=CYLINDRICAL_SURFACE('',#18973,8.175);
#16450=CYLINDRICAL_SURFACE('',#18974,8.175);
#16451=CYLINDRICAL_SURFACE('',#18975,8.175);
#16452=CYLINDRICAL_SURFACE('',#18976,8.175);
#16453=CYLINDRICAL_SURFACE('',#18977,8.175);
#16454=CYLINDRICAL_SURFACE('',#18978,8.175);
#16455=CYLINDRICAL_SURFACE('',#18979,8.175);
#16456=CYLINDRICAL_SURFACE('',#18980,8.175);
#16457=CYLINDRICAL_SURFACE('',#18981,8.175);
#16458=CYLINDRICAL_SURFACE('',#18982,8.175);
#16459=CYLINDRICAL_SURFACE('',#18983,8.175);
#16460=CYLINDRICAL_SURFACE('',#18984,8.175);
#16461=CYLINDRICAL_SURFACE('',#18985,8.175);
#16462=CYLINDRICAL_SURFACE('',#18986,8.175);
#16463=CYLINDRICAL_SURFACE('',#18987,8.175);
#16464=CYLINDRICAL_SURFACE('',#18988,8.175);
#16465=CYLINDRICAL_SURFACE('',#18989,8.175);
#16466=CYLINDRICAL_SURFACE('',#18990,8.175);
#16467=CYLINDRICAL_SURFACE('',#18991,8.175);
#16468=CYLINDRICAL_SURFACE('',#18992,8.175);
#16469=CYLINDRICAL_SURFACE('',#18993,8.175);
#16470=CYLINDRICAL_SURFACE('',#18994,8.175);
#16471=CYLINDRICAL_SURFACE('',#18995,8.175);
#16472=CYLINDRICAL_SURFACE('',#18996,8.175);
#16473=CYLINDRICAL_SURFACE('',#18997,8.175);
#16474=CYLINDRICAL_SURFACE('',#18998,8.175);
#16475=CYLINDRICAL_SURFACE('',#18999,8.175);
#16476=CYLINDRICAL_SURFACE('',#19000,8.175);
#16477=CYLINDRICAL_SURFACE('',#19001,8.175);
#16478=CYLINDRICAL_SURFACE('',#19002,8.175);
#16479=CYLINDRICAL_SURFACE('',#19003,8.175);
#16480=CYLINDRICAL_SURFACE('',#19004,8.175);
#16481=CYLINDRICAL_SURFACE('',#19005,8.175);
#16482=CYLINDRICAL_SURFACE('',#19006,8.175);
#16483=CYLINDRICAL_SURFACE('',#19007,8.175);
#16484=CYLINDRICAL_SURFACE('',#19008,8.175);
#16485=CYLINDRICAL_SURFACE('',#19009,8.175);
#16486=CYLINDRICAL_SURFACE('',#19010,8.175);
#16487=CYLINDRICAL_SURFACE('',#19011,8.175);
#16488=CYLINDRICAL_SURFACE('',#19012,8.175);
#16489=CYLINDRICAL_SURFACE('',#19013,8.175);
#16490=CYLINDRICAL_SURFACE('',#19014,8.175);
#16491=CYLINDRICAL_SURFACE('',#19015,8.175);
#16492=CYLINDRICAL_SURFACE('',#19016,8.175);
#16493=CYLINDRICAL_SURFACE('',#19017,8.175);
#16494=CYLINDRICAL_SURFACE('',#19018,8.175);
#16495=CYLINDRICAL_SURFACE('',#19019,8.175);
#16496=CYLINDRICAL_SURFACE('',#19020,8.175);
#16497=CYLINDRICAL_SURFACE('',#19021,8.175);
#16498=CYLINDRICAL_SURFACE('',#19022,8.175);
#16499=CYLINDRICAL_SURFACE('',#19023,8.175);
#16500=CYLINDRICAL_SURFACE('',#19024,8.175);
#16501=CYLINDRICAL_SURFACE('',#19025,8.175);
#16502=CYLINDRICAL_SURFACE('',#19026,8.175);
#16503=CYLINDRICAL_SURFACE('',#19027,8.175);
#16504=CYLINDRICAL_SURFACE('',#19028,8.175);
#16505=CYLINDRICAL_SURFACE('',#19029,8.175);
#16506=CYLINDRICAL_SURFACE('',#19030,8.175);
#16507=CYLINDRICAL_SURFACE('',#19032,8.175);
#16508=CYLINDRICAL_SURFACE('',#19200,1.5);
#16509=CYLINDRICAL_SURFACE('',#19224,2.);
#16510=CYLINDRICAL_SURFACE('',#19233,2.);
#16511=CYLINDRICAL_SURFACE('',#19242,2.);
#16512=CYLINDRICAL_SURFACE('',#19251,2.);
#16513=CYLINDRICAL_SURFACE('',#19260,2.);
#16514=CYLINDRICAL_SURFACE('',#19269,2.);
#16515=CYLINDRICAL_SURFACE('',#19278,2.);
#16516=CYLINDRICAL_SURFACE('',#19287,2.);
#16517=CYLINDRICAL_SURFACE('',#19296,2.);
#16518=CYLINDRICAL_SURFACE('',#19305,2.);
#16519=CYLINDRICAL_SURFACE('',#19314,2.);
#16520=CYLINDRICAL_SURFACE('',#19323,2.);
#16521=CYLINDRICAL_SURFACE('',#19332,4.);
#16522=CYLINDRICAL_SURFACE('',#19492,2.);
#16523=CYLINDRICAL_SURFACE('',#19494,8.175);
#16524=CYLINDRICAL_SURFACE('',#19495,8.175);
#16525=CYLINDRICAL_SURFACE('',#19496,8.175);
#16526=CYLINDRICAL_SURFACE('',#19497,8.175);
#16527=CYLINDRICAL_SURFACE('',#19498,8.175);
#16528=CYLINDRICAL_SURFACE('',#19499,8.175);
#16529=CYLINDRICAL_SURFACE('',#19500,8.175);
#16530=CYLINDRICAL_SURFACE('',#19501,8.175);
#16531=CYLINDRICAL_SURFACE('',#19502,8.175);
#16532=CYLINDRICAL_SURFACE('',#19503,8.175);
#16533=CYLINDRICAL_SURFACE('',#19504,8.175);
#16534=CYLINDRICAL_SURFACE('',#19505,8.175);
#16535=CYLINDRICAL_SURFACE('',#19506,8.175);
#16536=CYLINDRICAL_SURFACE('',#19507,8.175);
#16537=CYLINDRICAL_SURFACE('',#19508,8.175);
#16538=CYLINDRICAL_SURFACE('',#19509,8.175);
#16539=CYLINDRICAL_SURFACE('',#19510,8.175);
#16540=CYLINDRICAL_SURFACE('',#19511,8.175);
#16541=CYLINDRICAL_SURFACE('',#19512,8.175);
#16542=CYLINDRICAL_SURFACE('',#19513,8.175);
#16543=CYLINDRICAL_SURFACE('',#19514,8.175);
#16544=CYLINDRICAL_SURFACE('',#19515,8.175);
#16545=CYLINDRICAL_SURFACE('',#19516,8.175);
#16546=CYLINDRICAL_SURFACE('',#19517,8.175);
#16547=CYLINDRICAL_SURFACE('',#19518,8.175);
#16548=CYLINDRICAL_SURFACE('',#19519,8.175);
#16549=CYLINDRICAL_SURFACE('',#19520,8.175);
#16550=CYLINDRICAL_SURFACE('',#19521,8.175);
#16551=CYLINDRICAL_SURFACE('',#19522,8.175);
#16552=CYLINDRICAL_SURFACE('',#19523,8.175);
#16553=CYLINDRICAL_SURFACE('',#19524,8.175);
#16554=CYLINDRICAL_SURFACE('',#19525,8.175);
#16555=CYLINDRICAL_SURFACE('',#19526,8.175);
#16556=CYLINDRICAL_SURFACE('',#19527,8.175);
#16557=CYLINDRICAL_SURFACE('',#19528,8.175);
#16558=CYLINDRICAL_SURFACE('',#19529,8.175);
#16559=CYLINDRICAL_SURFACE('',#19530,8.175);
#16560=CYLINDRICAL_SURFACE('',#19531,8.175);
#16561=CYLINDRICAL_SURFACE('',#19532,8.175);
#16562=CYLINDRICAL_SURFACE('',#19533,8.175);
#16563=CYLINDRICAL_SURFACE('',#19534,8.175);
#16564=CYLINDRICAL_SURFACE('',#19535,8.175);
#16565=CYLINDRICAL_SURFACE('',#19536,8.175);
#16566=CYLINDRICAL_SURFACE('',#19537,8.175);
#16567=CYLINDRICAL_SURFACE('',#19538,8.175);
#16568=CYLINDRICAL_SURFACE('',#19539,8.175);
#16569=CYLINDRICAL_SURFACE('',#19540,8.175);
#16570=CYLINDRICAL_SURFACE('',#19541,8.175);
#16571=CYLINDRICAL_SURFACE('',#19542,8.175);
#16572=CYLINDRICAL_SURFACE('',#19543,8.175);
#16573=CYLINDRICAL_SURFACE('',#19544,8.175);
#16574=CYLINDRICAL_SURFACE('',#19545,8.175);
#16575=CYLINDRICAL_SURFACE('',#19546,8.175);
#16576=CYLINDRICAL_SURFACE('',#19547,8.175);
#16577=CYLINDRICAL_SURFACE('',#19548,8.175);
#16578=CYLINDRICAL_SURFACE('',#19549,8.175);
#16579=CYLINDRICAL_SURFACE('',#19550,8.175);
#16580=CYLINDRICAL_SURFACE('',#19551,8.175);
#16581=CYLINDRICAL_SURFACE('',#19552,8.175);
#16582=CYLINDRICAL_SURFACE('',#19553,8.175);
#16583=CYLINDRICAL_SURFACE('',#19554,8.175);
#16584=CYLINDRICAL_SURFACE('',#19555,8.175);
#16585=CYLINDRICAL_SURFACE('',#19556,8.175);
#16586=CYLINDRICAL_SURFACE('',#19557,8.175);
#16587=CYLINDRICAL_SURFACE('',#19558,8.175);
#16588=CYLINDRICAL_SURFACE('',#19559,8.175);
#16589=CYLINDRICAL_SURFACE('',#19560,8.175);
#16590=CYLINDRICAL_SURFACE('',#19561,8.175);
#16591=CYLINDRICAL_SURFACE('',#19562,8.175);
#16592=CYLINDRICAL_SURFACE('',#19563,8.175);
#16593=CYLINDRICAL_SURFACE('',#19564,8.175);
#16594=CYLINDRICAL_SURFACE('',#19565,8.175);
#16595=CYLINDRICAL_SURFACE('',#19566,8.175);
#16596=CYLINDRICAL_SURFACE('',#19567,8.175);
#16597=CYLINDRICAL_SURFACE('',#19568,8.175);
#16598=CYLINDRICAL_SURFACE('',#19569,8.175);
#16599=CYLINDRICAL_SURFACE('',#19571,8.175);
#16600=ADVANCED_FACE('',(#1641),#16245,.T.);
#16601=ADVANCED_FACE('',(#1642),#16246,.T.);
#16602=ADVANCED_FACE('',(#1643),#1192,.F.);
#16603=ADVANCED_FACE('',(#1644),#1193,.F.);
#16604=ADVANCED_FACE('',(#1645),#1194,.F.);
#16605=ADVANCED_FACE('',(#1646),#1195,.T.);
#16606=ADVANCED_FACE('',(#1647),#16247,.F.);
#16607=ADVANCED_FACE('',(#1648),#1196,.T.);
#16608=ADVANCED_FACE('',(#1649),#1197,.T.);
#16609=ADVANCED_FACE('',(#1650),#16248,.T.);
#16610=ADVANCED_FACE('',(#1651),#16249,.T.);
#16611=ADVANCED_FACE('',(#1652),#16250,.F.);
#16612=ADVANCED_FACE('',(#1653),#16251,.T.);
#16613=ADVANCED_FACE('',(#1654),#1198,.F.);
#16614=ADVANCED_FACE('',(#1655),#1199,.F.);
#16615=ADVANCED_FACE('',(#1656),#1200,.F.);
#16616=ADVANCED_FACE('',(#1657),#1201,.T.);
#16617=ADVANCED_FACE('',(#1658),#1202,.T.);
#16618=ADVANCED_FACE('',(#1659),#16252,.T.);
#16619=ADVANCED_FACE('',(#1660),#1203,.T.);
#16620=ADVANCED_FACE('',(#1661),#1204,.T.);
#16621=ADVANCED_FACE('',(#1662),#1205,.T.);
#16622=ADVANCED_FACE('',(#1663),#1206,.T.);
#16623=ADVANCED_FACE('',(#1664),#1207,.F.);
#16624=ADVANCED_FACE('',(#1665),#1208,.T.);
#16625=ADVANCED_FACE('',(#1666),#16253,.F.);
#16626=ADVANCED_FACE('',(#1667),#1209,.T.);
#16627=ADVANCED_FACE('',(#1668),#16254,.T.);
#16628=ADVANCED_FACE('',(#1669),#1210,.T.);
#16629=ADVANCED_FACE('',(#1670),#16255,.T.);
#16630=ADVANCED_FACE('',(#1671),#1211,.T.);
#16631=ADVANCED_FACE('',(#1672),#1212,.T.);
#16632=ADVANCED_FACE('',(#1673),#1213,.T.);
#16633=ADVANCED_FACE('',(#1674),#1214,.F.);
#16634=ADVANCED_FACE('',(#1675),#1215,.T.);
#16635=ADVANCED_FACE('',(#1676),#16256,.F.);
#16636=ADVANCED_FACE('',(#1677),#1216,.T.);
#16637=ADVANCED_FACE('',(#1678),#16257,.T.);
#16638=ADVANCED_FACE('',(#1679),#1217,.T.);
#16639=ADVANCED_FACE('',(#1680),#16258,.T.);
#16640=ADVANCED_FACE('',(#1681),#16259,.T.);
#16641=ADVANCED_FACE('',(#1682),#1218,.F.);
#16642=ADVANCED_FACE('',(#1683),#1219,.F.);
#16643=ADVANCED_FACE('',(#1684),#1220,.T.);
#16644=ADVANCED_FACE('',(#1685),#1221,.T.);
#16645=ADVANCED_FACE('',(#1686),#16260,.T.);
#16646=ADVANCED_FACE('',(#1687),#16261,.T.);
#16647=ADVANCED_FACE('',(#1688),#16262,.T.);
#16648=ADVANCED_FACE('',(#1689),#1222,.F.);
#16649=ADVANCED_FACE('',(#1690),#1223,.F.);
#16650=ADVANCED_FACE('',(#1691),#1224,.T.);
#16651=ADVANCED_FACE('',(#1692),#1225,.T.);
#16652=ADVANCED_FACE('',(#1693),#1226,.T.);
#16653=ADVANCED_FACE('',(#1694),#1227,.T.);
#16654=ADVANCED_FACE('',(#1695),#1228,.T.);
#16655=ADVANCED_FACE('',(#1696),#1229,.T.);
#16656=ADVANCED_FACE('',(#1697),#1230,.T.);
#16657=ADVANCED_FACE('',(#1698),#1231,.F.);
#16658=ADVANCED_FACE('',(#1699),#16263,.T.);
#16659=ADVANCED_FACE('',(#1700),#1232,.T.);
#16660=ADVANCED_FACE('',(#1701),#1233,.T.);
#16661=ADVANCED_FACE('',(#1702),#16264,.T.);
#16662=ADVANCED_FACE('',(#1703),#1018,.F.);
#16663=ADVANCED_FACE('',(#1704),#16265,.F.);
#16664=ADVANCED_FACE('',(#1705),#1019,.T.);
#16665=ADVANCED_FACE('',(#1706),#1020,.T.);
#16666=ADVANCED_FACE('',(#1707,#862),#16266,.T.);
#16667=ADVANCED_FACE('',(#1708),#1021,.T.);
#16668=ADVANCED_FACE('',(#1709,#863),#1234,.T.);
#16669=ADVANCED_FACE('',(#1710),#1235,.F.);
#16670=ADVANCED_FACE('',(#1711),#1236,.T.);
#16671=ADVANCED_FACE('',(#1712),#16267,.F.);
#16672=ADVANCED_FACE('',(#1713),#16268,.F.);
#16673=ADVANCED_FACE('',(#1714),#16269,.F.);
#16674=ADVANCED_FACE('',(#1715),#16270,.F.);
#16675=ADVANCED_FACE('',(#1716),#16271,.F.);
#16676=ADVANCED_FACE('',(#1717),#16272,.F.);
#16677=ADVANCED_FACE('',(#1718),#16273,.F.);
#16678=ADVANCED_FACE('',(#1719),#16274,.F.);
#16679=ADVANCED_FACE('',(#1720),#16275,.F.);
#16680=ADVANCED_FACE('',(#1721),#16276,.F.);
#16681=ADVANCED_FACE('',(#1722),#16277,.F.);
#16682=ADVANCED_FACE('',(#1723),#16278,.F.);
#16683=ADVANCED_FACE('',(#1724),#16279,.F.);
#16684=ADVANCED_FACE('',(#1725),#16280,.F.);
#16685=ADVANCED_FACE('',(#1726),#16281,.F.);
#16686=ADVANCED_FACE('',(#1727),#16282,.F.);
#16687=ADVANCED_FACE('',(#1728),#16283,.F.);
#16688=ADVANCED_FACE('',(#1729),#16284,.F.);
#16689=ADVANCED_FACE('',(#1730),#16285,.F.);
#16690=ADVANCED_FACE('',(#1731),#16286,.F.);
#16691=ADVANCED_FACE('',(#1732),#16287,.F.);
#16692=ADVANCED_FACE('',(#1733),#16288,.F.);
#16693=ADVANCED_FACE('',(#1734),#16289,.F.);
#16694=ADVANCED_FACE('',(#1735),#16290,.F.);
#16695=ADVANCED_FACE('',(#1736),#16291,.F.);
#16696=ADVANCED_FACE('',(#1737),#16292,.F.);
#16697=ADVANCED_FACE('',(#1738),#16293,.F.);
#16698=ADVANCED_FACE('',(#1739),#16294,.F.);
#16699=ADVANCED_FACE('',(#1740),#16295,.F.);
#16700=ADVANCED_FACE('',(#1741),#16296,.F.);
#16701=ADVANCED_FACE('',(#1742),#16297,.F.);
#16702=ADVANCED_FACE('',(#1743),#16298,.F.);
#16703=ADVANCED_FACE('',(#1744),#16299,.F.);
#16704=ADVANCED_FACE('',(#1745),#16300,.F.);
#16705=ADVANCED_FACE('',(#1746),#16301,.F.);
#16706=ADVANCED_FACE('',(#1747),#16302,.F.);
#16707=ADVANCED_FACE('',(#1748),#16303,.F.);
#16708=ADVANCED_FACE('',(#1749),#16304,.F.);
#16709=ADVANCED_FACE('',(#1750),#16305,.F.);
#16710=ADVANCED_FACE('',(#1751),#16306,.F.);
#16711=ADVANCED_FACE('',(#1752),#16307,.F.);
#16712=ADVANCED_FACE('',(#1753),#16308,.F.);
#16713=ADVANCED_FACE('',(#1754),#16309,.F.);
#16714=ADVANCED_FACE('',(#1755),#16310,.F.);
#16715=ADVANCED_FACE('',(#1756),#16311,.F.);
#16716=ADVANCED_FACE('',(#1757),#16312,.F.);
#16717=ADVANCED_FACE('',(#1758),#16313,.F.);
#16718=ADVANCED_FACE('',(#1759),#16314,.F.);
#16719=ADVANCED_FACE('',(#1760),#16315,.F.);
#16720=ADVANCED_FACE('',(#1761),#16316,.F.);
#16721=ADVANCED_FACE('',(#1762),#1022,.F.);
#16722=ADVANCED_FACE('',(#1763),#16317,.F.);
#16723=ADVANCED_FACE('',(#1764),#140,.T.);
#16724=ADVANCED_FACE('',(#1765),#16318,.T.);
#16725=ADVANCED_FACE('',(#1766),#141,.T.);
#16726=ADVANCED_FACE('',(#1767),#16319,.T.);
#16727=ADVANCED_FACE('',(#1768),#16320,.F.);
#16728=ADVANCED_FACE('',(#1769),#16321,.F.);
#16729=ADVANCED_FACE('',(#1770,#864),#1237,.T.);
#16730=ADVANCED_FACE('',(#1771,#865),#1238,.T.);
#16731=ADVANCED_FACE('',(#1772,#866),#1239,.T.);
#16732=ADVANCED_FACE('',(#1773,#867),#1240,.T.);
#16733=ADVANCED_FACE('',(#1774,#868),#1241,.T.);
#16734=ADVANCED_FACE('',(#1775),#138,.F.);
#16735=ADVANCED_FACE('',(#1776),#1242,.F.);
#16736=ADVANCED_FACE('',(#1777),#139,.F.);
#16737=ADVANCED_FACE('',(#1778),#1243,.T.);
#16738=ADVANCED_FACE('',(#1779),#1244,.F.);
#16739=ADVANCED_FACE('',(#1780),#16322,.F.);
#16740=ADVANCED_FACE('',(#1781),#124,.T.);
#16741=ADVANCED_FACE('',(#1782),#125,.T.);
#16742=ADVANCED_FACE('',(#1783),#16323,.F.);
#16743=ADVANCED_FACE('',(#1784),#16324,.T.);
#16744=ADVANCED_FACE('',(#1785),#1245,.F.);
#16745=ADVANCED_FACE('',(#1786,#869),#1246,.T.);
#16746=ADVANCED_FACE('',(#1787),#1247,.T.);
#16747=ADVANCED_FACE('',(#1788),#16325,.F.);
#16748=ADVANCED_FACE('',(#1789),#16326,.T.);
#16749=ADVANCED_FACE('',(#1790,#870),#1248,.T.);
#16750=ADVANCED_FACE('',(#1791,#871),#1249,.F.);
#16751=ADVANCED_FACE('',(#1792),#142,.T.);
#16752=ADVANCED_FACE('',(#1793),#143,.T.);
#16753=ADVANCED_FACE('',(#1794),#16327,.T.);
#16754=ADVANCED_FACE('',(#1795),#16328,.T.);
#16755=ADVANCED_FACE('',(#1796),#1250,.F.);
#16756=ADVANCED_FACE('',(#1797),#1251,.F.);
#16757=ADVANCED_FACE('',(#1798),#144,.T.);
#16758=ADVANCED_FACE('',(#1799),#16329,.T.);
#16759=ADVANCED_FACE('',(#1800),#1023,.T.);
#16760=ADVANCED_FACE('',(#1801),#16330,.T.);
#16761=ADVANCED_FACE('',(#1802),#1024,.T.);
#16762=ADVANCED_FACE('',(#1803,#872),#78,.T.);
#16763=ADVANCED_FACE('',(#1804),#16331,.T.);
#16764=ADVANCED_FACE('',(#1805,#873),#1252,.T.);
#16765=ADVANCED_FACE('',(#1806),#1253,.T.);
#16766=ADVANCED_FACE('',(#1807,#874),#1254,.T.);
#16767=ADVANCED_FACE('',(#1808),#1025,.T.);
#16768=ADVANCED_FACE('',(#1809),#79,.T.);
#16769=ADVANCED_FACE('',(#1810),#145,.T.);
#16770=ADVANCED_FACE('',(#1811),#16332,.F.);
#16771=ADVANCED_FACE('',(#1812),#146,.T.);
#16772=ADVANCED_FACE('',(#1813),#80,.F.);
#16773=ADVANCED_FACE('',(#1814),#1026,.T.);
#16774=ADVANCED_FACE('',(#1815),#81,.T.);
#16775=ADVANCED_FACE('',(#1816),#16333,.F.);
#16776=ADVANCED_FACE('',(#1817,#875),#1255,.F.);
#16777=ADVANCED_FACE('',(#1818),#1256,.T.);
#16778=ADVANCED_FACE('',(#1819),#1257,.T.);
#16779=ADVANCED_FACE('',(#1820),#16334,.F.);
#16780=ADVANCED_FACE('',(#1821),#16335,.T.);
#16781=ADVANCED_FACE('',(#1822),#16336,.T.);
#16782=ADVANCED_FACE('',(#1823),#1258,.F.);
#16783=ADVANCED_FACE('',(#1824),#1259,.F.);
#16784=ADVANCED_FACE('',(#1825),#126,.T.);
#16785=ADVANCED_FACE('',(#1826),#127,.T.);
#16786=ADVANCED_FACE('',(#1827),#128,.T.);
#16787=ADVANCED_FACE('',(#1828),#82,.T.);
#16788=ADVANCED_FACE('',(#1829),#16337,.T.);
#16789=ADVANCED_FACE('',(#1830),#83,.T.);
#16790=ADVANCED_FACE('',(#1831),#147,.T.);
#16791=ADVANCED_FACE('',(#1832),#84,.T.);
#16792=ADVANCED_FACE('',(#1833),#129,.T.);
#16793=ADVANCED_FACE('',(#1834),#130,.T.);
#16794=ADVANCED_FACE('',(#1835),#131,.T.);
#16795=ADVANCED_FACE('',(#1836),#85,.T.);
#16796=ADVANCED_FACE('',(#1837),#148,.T.);
#16797=ADVANCED_FACE('',(#1838),#16338,.T.);
#16798=ADVANCED_FACE('',(#1839),#86,.T.);
#16799=ADVANCED_FACE('',(#1840),#132,.T.);
#16800=ADVANCED_FACE('',(#1841),#133,.T.);
#16801=ADVANCED_FACE('',(#1842),#134,.T.);
#16802=ADVANCED_FACE('',(#1843),#87,.T.);
#16803=ADVANCED_FACE('',(#1844),#16339,.F.);
#16804=ADVANCED_FACE('',(#1845),#88,.T.);
#16805=ADVANCED_FACE('',(#1846),#1027,.T.);
#16806=ADVANCED_FACE('',(#1847),#16340,.T.);
#16807=ADVANCED_FACE('',(#1848),#1028,.T.);
#16808=ADVANCED_FACE('',(#1849),#1260,.F.);
#16809=ADVANCED_FACE('',(#1850,#876),#1261,.F.);
#16810=ADVANCED_FACE('',(#1851,#877),#1262,.F.);
#16811=ADVANCED_FACE('',(#1852),#149,.T.);
#16812=ADVANCED_FACE('',(#1853),#16341,.F.);
#16813=ADVANCED_FACE('',(#1854),#1029,.T.);
#16814=ADVANCED_FACE('',(#1855),#150,.T.);
#16815=ADVANCED_FACE('',(#1856),#89,.F.);
#16816=ADVANCED_FACE('',(#1857),#16342,.F.);
#16817=ADVANCED_FACE('',(#1858),#1030,.T.);
#16818=ADVANCED_FACE('',(#1859),#90,.T.);
#16819=ADVANCED_FACE('',(#1860,#878),#1263,.F.);
#16820=ADVANCED_FACE('',(#1861),#1264,.F.);
#16821=ADVANCED_FACE('',(#1862),#1265,.F.);
#16822=ADVANCED_FACE('',(#1863),#1266,.F.);
#16823=ADVANCED_FACE('',(#1864),#1267,.F.);
#16824=ADVANCED_FACE('',(#1865),#135,.T.);
#16825=ADVANCED_FACE('',(#1866),#151,.T.);
#16826=ADVANCED_FACE('',(#1867),#152,.T.);
#16827=ADVANCED_FACE('',(#1868),#136,.T.);
#16828=ADVANCED_FACE('',(#1869),#153,.T.);
#16829=ADVANCED_FACE('',(#1870),#137,.T.);
#16830=ADVANCED_FACE('',(#1871),#91,.T.);
#16831=ADVANCED_FACE('',(#1872),#16343,.F.);
#16832=ADVANCED_FACE('',(#1873),#92,.T.);
#16833=ADVANCED_FACE('',(#1874),#1031,.T.);
#16834=ADVANCED_FACE('',(#1875),#16344,.T.);
#16835=ADVANCED_FACE('',(#1876),#1032,.T.);
#16836=ADVANCED_FACE('',(#1877),#1268,.F.);
#16837=ADVANCED_FACE('',(#1878,#879),#1269,.F.);
#16838=ADVANCED_FACE('',(#1879,#880),#1270,.F.);
#16839=ADVANCED_FACE('',(#1880),#154,.T.);
#16840=ADVANCED_FACE('',(#1881),#1033,.T.);
#16841=ADVANCED_FACE('',(#1882),#16345,.T.);
#16842=ADVANCED_FACE('',(#1883),#1034,.T.);
#16843=ADVANCED_FACE('',(#1884),#16346,.T.);
#16844=ADVANCED_FACE('',(#1885),#16347,.T.);
#16845=ADVANCED_FACE('',(#1886),#16348,.T.);
#16846=ADVANCED_FACE('',(#1887),#1271,.F.);
#16847=ADVANCED_FACE('',(#1888,#881),#1272,.F.);
#16848=ADVANCED_FACE('',(#1889,#882),#1273,.F.);
#16849=ADVANCED_FACE('',(#1890),#1274,.F.);
#16850=ADVANCED_FACE('',(#1891),#155,.T.);
#16851=ADVANCED_FACE('',(#1892),#16349,.T.);
#16852=ADVANCED_FACE('',(#1893),#156,.T.);
#16853=ADVANCED_FACE('',(#1894),#157,.T.);
#16854=ADVANCED_FACE('',(#1895),#16350,.T.);
#16855=ADVANCED_FACE('',(#1896),#158,.T.);
#16856=ADVANCED_FACE('',(#1897),#16351,.T.);
#16857=ADVANCED_FACE('',(#1898),#159,.T.);
#16858=ADVANCED_FACE('',(#1899),#160,.T.);
#16859=ADVANCED_FACE('',(#1900),#16352,.T.);
#16860=ADVANCED_FACE('',(#1901),#16353,.F.);
#16861=ADVANCED_FACE('',(#1902),#16354,.F.);
#16862=ADVANCED_FACE('',(#1903),#16355,.F.);
#16863=ADVANCED_FACE('',(#1904),#16356,.F.);
#16864=ADVANCED_FACE('',(#1905),#16357,.T.);
#16865=ADVANCED_FACE('',(#1906),#16358,.T.);
#16866=ADVANCED_FACE('',(#1907),#16359,.T.);
#16867=ADVANCED_FACE('',(#1908),#16360,.T.);
#16868=ADVANCED_FACE('',(#1909),#16361,.T.);
#16869=ADVANCED_FACE('',(#1910),#16362,.T.);
#16870=ADVANCED_FACE('',(#1911),#161,.T.);
#16871=ADVANCED_FACE('',(#1912),#162,.T.);
#16872=ADVANCED_FACE('',(#1913),#163,.T.);
#16873=ADVANCED_FACE('',(#1914),#164,.T.);
#16874=ADVANCED_FACE('',(#1915),#165,.T.);
#16875=ADVANCED_FACE('',(#1916),#166,.T.);
#16876=ADVANCED_FACE('',(#1917),#167,.T.);
#16877=ADVANCED_FACE('',(#1918),#168,.T.);
#16878=ADVANCED_FACE('',(#1919),#169,.T.);
#16879=ADVANCED_FACE('',(#1920),#170,.T.);
#16880=ADVANCED_FACE('',(#1921),#1275,.F.);
#16881=ADVANCED_FACE('',(#1922),#16363,.T.);
#16882=ADVANCED_FACE('',(#1923,#883),#1276,.F.);
#16883=ADVANCED_FACE('',(#1924,#884),#1277,.F.);
#16884=ADVANCED_FACE('',(#1925),#1278,.F.);
#16885=ADVANCED_FACE('',(#1926),#171,.T.);
#16886=ADVANCED_FACE('',(#1927),#172,.T.);
#16887=ADVANCED_FACE('',(#1928),#16364,.F.);
#16888=ADVANCED_FACE('',(#1929),#16365,.F.);
#16889=ADVANCED_FACE('',(#1930),#16366,.F.);
#16890=ADVANCED_FACE('',(#1931),#93,.T.);
#16891=ADVANCED_FACE('',(#1932),#94,.T.);
#16892=ADVANCED_FACE('',(#1933),#173,.T.);
#16893=ADVANCED_FACE('',(#1934),#95,.T.);
#16894=ADVANCED_FACE('',(#1935),#96,.T.);
#16895=ADVANCED_FACE('',(#1936),#16367,.T.);
#16896=ADVANCED_FACE('',(#1937),#16368,.T.);
#16897=ADVANCED_FACE('',(#1938),#97,.T.);
#16898=ADVANCED_FACE('',(#1939),#98,.T.);
#16899=ADVANCED_FACE('',(#1940),#174,.T.);
#16900=ADVANCED_FACE('',(#1941),#99,.T.);
#16901=ADVANCED_FACE('',(#1942),#100,.T.);
#16902=ADVANCED_FACE('',(#1943),#16369,.T.);
#16903=ADVANCED_FACE('',(#1944),#101,.T.);
#16904=ADVANCED_FACE('',(#1945),#102,.T.);
#16905=ADVANCED_FACE('',(#1946),#175,.T.);
#16906=ADVANCED_FACE('',(#1947),#103,.T.);
#16907=ADVANCED_FACE('',(#1948),#104,.T.);
#16908=ADVANCED_FACE('',(#1949),#176,.T.);
#16909=ADVANCED_FACE('',(#1950),#105,.T.);
#16910=ADVANCED_FACE('',(#1951),#106,.T.);
#16911=ADVANCED_FACE('',(#1952),#16370,.T.);
#16912=ADVANCED_FACE('',(#1953),#16371,.T.);
#16913=ADVANCED_FACE('',(#1954),#107,.T.);
#16914=ADVANCED_FACE('',(#1955),#108,.T.);
#16915=ADVANCED_FACE('',(#1956),#109,.T.);
#16916=ADVANCED_FACE('',(#1957),#110,.T.);
#16917=ADVANCED_FACE('',(#1958),#16372,.T.);
#16918=ADVANCED_FACE('',(#1959),#111,.T.);
#16919=ADVANCED_FACE('',(#1960),#112,.T.);
#16920=ADVANCED_FACE('',(#1961),#177,.T.);
#16921=ADVANCED_FACE('',(#1962),#113,.T.);
#16922=ADVANCED_FACE('',(#1963),#114,.T.);
#16923=ADVANCED_FACE('',(#1964),#16373,.T.);
#16924=ADVANCED_FACE('',(#1965),#16374,.T.);
#16925=ADVANCED_FACE('',(#1966),#115,.T.);
#16926=ADVANCED_FACE('',(#1967),#116,.T.);
#16927=ADVANCED_FACE('',(#1968),#178,.T.);
#16928=ADVANCED_FACE('',(#1969),#1035,.F.);
#16929=ADVANCED_FACE('',(#1970),#1036,.F.);
#16930=ADVANCED_FACE('',(#1971),#1037,.F.);
#16931=ADVANCED_FACE('',(#1972),#1038,.F.);
#16932=ADVANCED_FACE('',(#1973),#1039,.F.);
#16933=ADVANCED_FACE('',(#1974),#1040,.F.);
#16934=ADVANCED_FACE('',(#1975),#1041,.F.);
#16935=ADVANCED_FACE('',(#1976),#1042,.F.);
#16936=ADVANCED_FACE('',(#1977),#1043,.F.);
#16937=ADVANCED_FACE('',(#1978),#1044,.F.);
#16938=ADVANCED_FACE('',(#1979),#16375,.F.);
#16939=ADVANCED_FACE('',(#1980),#16376,.F.);
#16940=ADVANCED_FACE('',(#1981),#16377,.F.);
#16941=ADVANCED_FACE('',(#1982),#16378,.F.);
#16942=ADVANCED_FACE('',(#1983),#16379,.F.);
#16943=ADVANCED_FACE('',(#1984),#16380,.F.);
#16944=ADVANCED_FACE('',(#1985),#1279,.F.);
#16945=ADVANCED_FACE('',(#1986),#1280,.F.);
#16946=ADVANCED_FACE('',(#1987,#885,#886),#1281,.F.);
#16947=ADVANCED_FACE('',(#1988),#1282,.F.);
#16948=ADVANCED_FACE('',(#1989),#1283,.F.);
#16949=ADVANCED_FACE('',(#1990),#1284,.F.);
#16950=ADVANCED_FACE('',(#1991,#887,#888),#1285,.F.);
#16951=ADVANCED_FACE('',(#1992,#889),#1286,.F.);
#16952=ADVANCED_FACE('',(#1993,#890),#1287,.T.);
#16953=ADVANCED_FACE('',(#1994),#16381,.F.);
#16954=ADVANCED_FACE('',(#1995),#1288,.F.);
#16955=ADVANCED_FACE('',(#1996,#891),#1289,.F.);
#16956=ADVANCED_FACE('',(#1997),#16382,.F.);
#16957=ADVANCED_FACE('',(#1998),#1290,.F.);
#16958=ADVANCED_FACE('',(#1999),#1291,.F.);
#16959=ADVANCED_FACE('',(#2000),#1292,.F.);
#16960=ADVANCED_FACE('',(#2001),#1293,.F.);
#16961=ADVANCED_FACE('',(#2002),#1294,.F.);
#16962=ADVANCED_FACE('',(#2003),#1295,.F.);
#16963=ADVANCED_FACE('',(#2004,#892),#1296,.F.);
#16964=ADVANCED_FACE('',(#2005),#1297,.F.);
#16965=ADVANCED_FACE('',(#2006),#1298,.F.);
#16966=ADVANCED_FACE('',(#2007),#1299,.F.);
#16967=ADVANCED_FACE('',(#2008),#16383,.F.);
#16968=ADVANCED_FACE('',(#2009,#893),#1300,.F.);
#16969=ADVANCED_FACE('',(#2010),#1301,.F.);
#16970=ADVANCED_FACE('',(#2011),#16384,.F.);
#16971=ADVANCED_FACE('',(#2012),#16385,.T.);
#16972=ADVANCED_FACE('',(#2013),#16386,.T.);
#16973=ADVANCED_FACE('',(#2014),#16387,.T.);
#16974=ADVANCED_FACE('',(#2015),#16388,.T.);
#16975=ADVANCED_FACE('',(#2016),#16389,.T.);
#16976=ADVANCED_FACE('',(#2017),#179,.T.);
#16977=ADVANCED_FACE('',(#2018),#117,.T.);
#16978=ADVANCED_FACE('',(#2019),#16390,.T.);
#16979=ADVANCED_FACE('',(#2020),#16391,.T.);
#16980=ADVANCED_FACE('',(#2021),#16392,.T.);
#16981=ADVANCED_FACE('',(#2022),#16393,.T.);
#16982=ADVANCED_FACE('',(#2023),#16394,.T.);
#16983=ADVANCED_FACE('',(#2024),#16395,.T.);
#16984=ADVANCED_FACE('',(#2025),#180,.T.);
#16985=ADVANCED_FACE('',(#2026),#118,.T.);
#16986=ADVANCED_FACE('',(#2027),#119,.T.);
#16987=ADVANCED_FACE('',(#2028),#16396,.T.);
#16988=ADVANCED_FACE('',(#2029),#16397,.T.);
#16989=ADVANCED_FACE('',(#2030),#16398,.T.);
#16990=ADVANCED_FACE('',(#2031),#16399,.T.);
#16991=ADVANCED_FACE('',(#2032),#120,.T.);
#16992=ADVANCED_FACE('',(#2033),#16400,.T.);
#16993=ADVANCED_FACE('',(#2034),#121,.T.);
#16994=ADVANCED_FACE('',(#2035),#16401,.T.);
#16995=ADVANCED_FACE('',(#2036),#16402,.T.);
#16996=ADVANCED_FACE('',(#2037),#16403,.T.);
#16997=ADVANCED_FACE('',(#2038),#16404,.T.);
#16998=ADVANCED_FACE('',(#2039),#16405,.T.);
#16999=ADVANCED_FACE('',(#2040),#122,.T.);
#17000=ADVANCED_FACE('',(#2041),#1045,.F.);
#17001=ADVANCED_FACE('',(#2042),#1046,.F.);
#17002=ADVANCED_FACE('',(#2043),#1047,.F.);
#17003=ADVANCED_FACE('',(#2044),#1048,.F.);
#17004=ADVANCED_FACE('',(#2045),#181,.T.);
#17005=ADVANCED_FACE('',(#2046),#182,.T.);
#17006=ADVANCED_FACE('',(#2047),#16406,.T.);
#17007=ADVANCED_FACE('',(#2048),#1302,.T.);
#17008=ADVANCED_FACE('',(#2049),#1303,.F.);
#17009=ADVANCED_FACE('',(#2050),#16407,.T.);
#17010=ADVANCED_FACE('',(#2051),#16408,.T.);
#17011=ADVANCED_FACE('',(#2052),#16409,.F.);
#17012=ADVANCED_FACE('',(#2053),#16410,.F.);
#17013=ADVANCED_FACE('',(#2054),#16411,.F.);
#17014=ADVANCED_FACE('',(#2055),#16412,.F.);
#17015=ADVANCED_FACE('',(#2056),#1304,.F.);
#17016=ADVANCED_FACE('',(#2057),#16413,.T.);
#17017=ADVANCED_FACE('',(#2058),#1305,.F.);
#17018=ADVANCED_FACE('',(#2059,#894),#1306,.F.);
#17019=ADVANCED_FACE('',(#2060,#895),#1307,.T.);
#17020=ADVANCED_FACE('',(#2061),#1308,.F.);
#17021=ADVANCED_FACE('',(#2062,#896),#1309,.F.);
#17022=ADVANCED_FACE('',(#2063),#16414,.T.);
#17023=ADVANCED_FACE('',(#2064),#1310,.F.);
#17024=ADVANCED_FACE('',(#2065,#897),#1311,.F.);
#17025=ADVANCED_FACE('',(#2066,#898),#1312,.F.);
#17026=ADVANCED_FACE('',(#2067,#899),#1313,.F.);
#17027=ADVANCED_FACE('',(#2068),#1314,.F.);
#17028=ADVANCED_FACE('',(#2069,#900),#1315,.T.);
#17029=ADVANCED_FACE('',(#2070,#901),#1316,.T.);
#17030=ADVANCED_FACE('',(#2071),#1317,.T.);
#17031=ADVANCED_FACE('',(#2072),#16415,.F.);
#17032=ADVANCED_FACE('',(#2073,#902),#123,.T.);
#17033=ADVANCED_FACE('',(#2074),#1318,.T.);
#17034=ADVANCED_FACE('',(#2075),#183,.F.);
#17035=ADVANCED_FACE('',(#2076),#1049,.T.);
#17036=ADVANCED_FACE('',(#2077),#1050,.T.);
#17037=ADVANCED_FACE('',(#2078),#1051,.T.);
#17038=ADVANCED_FACE('',(#2079),#16416,.T.);
#17039=ADVANCED_FACE('',(#2080),#1052,.T.);
#17040=ADVANCED_FACE('',(#2081),#1053,.T.);
#17041=ADVANCED_FACE('',(#2082),#16417,.T.);
#17042=ADVANCED_FACE('',(#2083),#1054,.T.);
#17043=ADVANCED_FACE('',(#2084),#1055,.T.);
#17044=ADVANCED_FACE('',(#2085),#16418,.T.);
#17045=ADVANCED_FACE('',(#2086),#1056,.T.);
#17046=ADVANCED_FACE('',(#2087),#1057,.T.);
#17047=ADVANCED_FACE('',(#2088),#16419,.T.);
#17048=ADVANCED_FACE('',(#2089),#1058,.T.);
#17049=ADVANCED_FACE('',(#2090),#1059,.T.);
#17050=ADVANCED_FACE('',(#2091),#16420,.T.);
#17051=ADVANCED_FACE('',(#2092),#1060,.T.);
#17052=ADVANCED_FACE('',(#2093),#1061,.T.);
#17053=ADVANCED_FACE('',(#2094),#16421,.T.);
#17054=ADVANCED_FACE('',(#2095),#1062,.T.);
#17055=ADVANCED_FACE('',(#2096),#1063,.T.);
#17056=ADVANCED_FACE('',(#2097),#16422,.T.);
#17057=ADVANCED_FACE('',(#2098),#1064,.T.);
#17058=ADVANCED_FACE('',(#2099),#1065,.T.);
#17059=ADVANCED_FACE('',(#2100),#16423,.T.);
#17060=ADVANCED_FACE('',(#2101),#1066,.T.);
#17061=ADVANCED_FACE('',(#2102),#1067,.T.);
#17062=ADVANCED_FACE('',(#2103),#16424,.T.);
#17063=ADVANCED_FACE('',(#2104),#1068,.T.);
#17064=ADVANCED_FACE('',(#2105),#1069,.T.);
#17065=ADVANCED_FACE('',(#2106),#16425,.T.);
#17066=ADVANCED_FACE('',(#2107),#1070,.T.);
#17067=ADVANCED_FACE('',(#2108),#1071,.T.);
#17068=ADVANCED_FACE('',(#2109),#16426,.T.);
#17069=ADVANCED_FACE('',(#2110),#1072,.T.);
#17070=ADVANCED_FACE('',(#2111),#1073,.T.);
#17071=ADVANCED_FACE('',(#2112),#16427,.T.);
#17072=ADVANCED_FACE('',(#2113),#1074,.T.);
#17073=ADVANCED_FACE('',(#2114),#1075,.T.);
#17074=ADVANCED_FACE('',(#2115),#16428,.T.);
#17075=ADVANCED_FACE('',(#2116),#1076,.T.);
#17076=ADVANCED_FACE('',(#2117),#1077,.T.);
#17077=ADVANCED_FACE('',(#2118),#16429,.T.);
#17078=ADVANCED_FACE('',(#2119),#1078,.T.);
#17079=ADVANCED_FACE('',(#2120),#1079,.T.);
#17080=ADVANCED_FACE('',(#2121),#1080,.T.);
#17081=ADVANCED_FACE('',(#2122),#1081,.T.);
#17082=ADVANCED_FACE('',(#2123),#16430,.T.);
#17083=ADVANCED_FACE('',(#2124),#16431,.T.);
#17084=ADVANCED_FACE('',(#2125),#16432,.T.);
#17085=ADVANCED_FACE('',(#2126),#16433,.T.);
#17086=ADVANCED_FACE('',(#2127),#16434,.T.);
#17087=ADVANCED_FACE('',(#2128),#16435,.T.);
#17088=ADVANCED_FACE('',(#2129),#16436,.T.);
#17089=ADVANCED_FACE('',(#2130),#16437,.T.);
#17090=ADVANCED_FACE('',(#2131),#16438,.T.);
#17091=ADVANCED_FACE('',(#2132),#16439,.T.);
#17092=ADVANCED_FACE('',(#2133),#16440,.T.);
#17093=ADVANCED_FACE('',(#2134),#16441,.T.);
#17094=ADVANCED_FACE('',(#2135),#16442,.T.);
#17095=ADVANCED_FACE('',(#2136),#16443,.T.);
#17096=ADVANCED_FACE('',(#2137),#16444,.T.);
#17097=ADVANCED_FACE('',(#2138),#16445,.T.);
#17098=ADVANCED_FACE('',(#2139),#16446,.T.);
#17099=ADVANCED_FACE('',(#2140),#16447,.T.);
#17100=ADVANCED_FACE('',(#2141),#16448,.T.);
#17101=ADVANCED_FACE('',(#2142),#16449,.T.);
#17102=ADVANCED_FACE('',(#2143),#16450,.T.);
#17103=ADVANCED_FACE('',(#2144),#16451,.T.);
#17104=ADVANCED_FACE('',(#2145),#16452,.T.);
#17105=ADVANCED_FACE('',(#2146),#16453,.T.);
#17106=ADVANCED_FACE('',(#2147),#16454,.T.);
#17107=ADVANCED_FACE('',(#2148),#16455,.T.);
#17108=ADVANCED_FACE('',(#2149),#16456,.T.);
#17109=ADVANCED_FACE('',(#2150),#16457,.T.);
#17110=ADVANCED_FACE('',(#2151),#16458,.T.);
#17111=ADVANCED_FACE('',(#2152),#16459,.T.);
#17112=ADVANCED_FACE('',(#2153),#16460,.T.);
#17113=ADVANCED_FACE('',(#2154),#16461,.T.);
#17114=ADVANCED_FACE('',(#2155),#16462,.T.);
#17115=ADVANCED_FACE('',(#2156),#16463,.T.);
#17116=ADVANCED_FACE('',(#2157),#16464,.T.);
#17117=ADVANCED_FACE('',(#2158),#16465,.T.);
#17118=ADVANCED_FACE('',(#2159),#16466,.T.);
#17119=ADVANCED_FACE('',(#2160),#16467,.T.);
#17120=ADVANCED_FACE('',(#2161),#16468,.T.);
#17121=ADVANCED_FACE('',(#2162),#16469,.T.);
#17122=ADVANCED_FACE('',(#2163),#16470,.T.);
#17123=ADVANCED_FACE('',(#2164),#16471,.T.);
#17124=ADVANCED_FACE('',(#2165),#16472,.T.);
#17125=ADVANCED_FACE('',(#2166),#16473,.T.);
#17126=ADVANCED_FACE('',(#2167),#16474,.T.);
#17127=ADVANCED_FACE('',(#2168),#16475,.T.);
#17128=ADVANCED_FACE('',(#2169),#16476,.T.);
#17129=ADVANCED_FACE('',(#2170),#16477,.T.);
#17130=ADVANCED_FACE('',(#2171),#16478,.T.);
#17131=ADVANCED_FACE('',(#2172),#16479,.T.);
#17132=ADVANCED_FACE('',(#2173),#16480,.T.);
#17133=ADVANCED_FACE('',(#2174),#16481,.T.);
#17134=ADVANCED_FACE('',(#2175),#16482,.T.);
#17135=ADVANCED_FACE('',(#2176),#16483,.T.);
#17136=ADVANCED_FACE('',(#2177),#16484,.T.);
#17137=ADVANCED_FACE('',(#2178),#16485,.T.);
#17138=ADVANCED_FACE('',(#2179),#16486,.T.);
#17139=ADVANCED_FACE('',(#2180),#16487,.T.);
#17140=ADVANCED_FACE('',(#2181),#16488,.T.);
#17141=ADVANCED_FACE('',(#2182),#16489,.T.);
#17142=ADVANCED_FACE('',(#2183),#16490,.T.);
#17143=ADVANCED_FACE('',(#2184),#16491,.T.);
#17144=ADVANCED_FACE('',(#2185),#16492,.T.);
#17145=ADVANCED_FACE('',(#2186),#16493,.T.);
#17146=ADVANCED_FACE('',(#2187),#16494,.T.);
#17147=ADVANCED_FACE('',(#2188),#16495,.T.);
#17148=ADVANCED_FACE('',(#2189),#16496,.T.);
#17149=ADVANCED_FACE('',(#2190),#16497,.T.);
#17150=ADVANCED_FACE('',(#2191),#16498,.T.);
#17151=ADVANCED_FACE('',(#2192),#16499,.T.);
#17152=ADVANCED_FACE('',(#2193),#16500,.T.);
#17153=ADVANCED_FACE('',(#2194),#16501,.T.);
#17154=ADVANCED_FACE('',(#2195),#16502,.T.);
#17155=ADVANCED_FACE('',(#2196),#16503,.T.);
#17156=ADVANCED_FACE('',(#2197),#16504,.T.);
#17157=ADVANCED_FACE('',(#2198),#16505,.T.);
#17158=ADVANCED_FACE('',(#2199),#16506,.T.);
#17159=ADVANCED_FACE('',(#2200,#903),#1319,.F.);
#17160=ADVANCED_FACE('',(#2201),#16507,.T.);
#17161=ADVANCED_FACE('',(#2202),#1320,.T.);
#17162=ADVANCED_FACE('',(#2203),#1321,.T.);
#17163=ADVANCED_FACE('',(#2204),#1322,.F.);
#17164=ADVANCED_FACE('',(#2205),#1323,.F.);
#17165=ADVANCED_FACE('',(#2206),#1324,.F.);
#17166=ADVANCED_FACE('',(#2207),#1325,.F.);
#17167=ADVANCED_FACE('',(#2208),#1326,.F.);
#17168=ADVANCED_FACE('',(#2209),#1327,.F.);
#17169=ADVANCED_FACE('',(#2210),#1328,.F.);
#17170=ADVANCED_FACE('',(#2211),#1329,.F.);
#17171=ADVANCED_FACE('',(#2212),#1330,.F.);
#17172=ADVANCED_FACE('',(#2213),#1331,.F.);
#17173=ADVANCED_FACE('',(#2214),#1332,.F.);
#17174=ADVANCED_FACE('',(#2215),#1333,.F.);
#17175=ADVANCED_FACE('',(#2216),#1334,.F.);
#17176=ADVANCED_FACE('',(#2217),#1335,.F.);
#17177=ADVANCED_FACE('',(#2218),#1336,.F.);
#17178=ADVANCED_FACE('',(#2219),#1337,.F.);
#17179=ADVANCED_FACE('',(#2220),#1338,.F.);
#17180=ADVANCED_FACE('',(#2221),#1339,.F.);
#17181=ADVANCED_FACE('',(#2222),#1340,.F.);
#17182=ADVANCED_FACE('',(#2223),#1341,.F.);
#17183=ADVANCED_FACE('',(#2224),#1342,.F.);
#17184=ADVANCED_FACE('',(#2225),#1343,.F.);
#17185=ADVANCED_FACE('',(#2226),#1344,.F.);
#17186=ADVANCED_FACE('',(#2227),#1345,.F.);
#17187=ADVANCED_FACE('',(#2228),#1346,.F.);
#17188=ADVANCED_FACE('',(#2229),#1347,.F.);
#17189=ADVANCED_FACE('',(#2230),#1348,.F.);
#17190=ADVANCED_FACE('',(#2231),#1349,.F.);
#17191=ADVANCED_FACE('',(#2232),#1350,.F.);
#17192=ADVANCED_FACE('',(#2233),#1351,.F.);
#17193=ADVANCED_FACE('',(#2234),#1352,.F.);
#17194=ADVANCED_FACE('',(#2235),#1353,.F.);
#17195=ADVANCED_FACE('',(#2236),#1354,.F.);
#17196=ADVANCED_FACE('',(#2237),#1355,.F.);
#17197=ADVANCED_FACE('',(#2238),#1356,.F.);
#17198=ADVANCED_FACE('',(#2239),#1357,.F.);
#17199=ADVANCED_FACE('',(#2240),#1358,.F.);
#17200=ADVANCED_FACE('',(#2241),#1359,.F.);
#17201=ADVANCED_FACE('',(#2242),#1360,.F.);
#17202=ADVANCED_FACE('',(#2243),#1361,.F.);
#17203=ADVANCED_FACE('',(#2244),#1362,.F.);
#17204=ADVANCED_FACE('',(#2245),#1363,.F.);
#17205=ADVANCED_FACE('',(#2246),#1364,.F.);
#17206=ADVANCED_FACE('',(#2247),#1365,.F.);
#17207=ADVANCED_FACE('',(#2248),#1366,.F.);
#17208=ADVANCED_FACE('',(#2249),#1367,.F.);
#17209=ADVANCED_FACE('',(#2250),#1368,.F.);
#17210=ADVANCED_FACE('',(#2251),#1369,.F.);
#17211=ADVANCED_FACE('',(#2252),#1370,.F.);
#17212=ADVANCED_FACE('',(#2253),#1371,.F.);
#17213=ADVANCED_FACE('',(#2254),#1372,.F.);
#17214=ADVANCED_FACE('',(#2255),#1373,.F.);
#17215=ADVANCED_FACE('',(#2256),#1374,.F.);
#17216=ADVANCED_FACE('',(#2257),#1375,.F.);
#17217=ADVANCED_FACE('',(#2258),#1376,.F.);
#17218=ADVANCED_FACE('',(#2259),#1377,.F.);
#17219=ADVANCED_FACE('',(#2260),#1378,.F.);
#17220=ADVANCED_FACE('',(#2261),#1379,.F.);
#17221=ADVANCED_FACE('',(#2262),#1380,.F.);
#17222=ADVANCED_FACE('',(#2263),#1381,.F.);
#17223=ADVANCED_FACE('',(#2264),#1382,.F.);
#17224=ADVANCED_FACE('',(#2265),#1383,.F.);
#17225=ADVANCED_FACE('',(#2266),#1384,.F.);
#17226=ADVANCED_FACE('',(#2267),#1385,.F.);
#17227=ADVANCED_FACE('',(#2268),#1386,.F.);
#17228=ADVANCED_FACE('',(#2269),#1387,.F.);
#17229=ADVANCED_FACE('',(#2270),#1388,.F.);
#17230=ADVANCED_FACE('',(#2271),#1389,.F.);
#17231=ADVANCED_FACE('',(#2272),#1390,.F.);
#17232=ADVANCED_FACE('',(#2273),#1391,.F.);
#17233=ADVANCED_FACE('',(#2274),#1392,.F.);
#17234=ADVANCED_FACE('',(#2275),#1393,.F.);
#17235=ADVANCED_FACE('',(#2276),#1394,.F.);
#17236=ADVANCED_FACE('',(#2277),#1395,.F.);
#17237=ADVANCED_FACE('',(#2278),#1396,.F.);
#17238=ADVANCED_FACE('',(#2279),#1397,.F.);
#17239=ADVANCED_FACE('',(#2280),#1398,.F.);
#17240=ADVANCED_FACE('',(#2281),#1399,.F.);
#17241=ADVANCED_FACE('',(#2282),#1400,.F.);
#17242=ADVANCED_FACE('',(#2283),#1401,.F.);
#17243=ADVANCED_FACE('',(#2284),#1402,.F.);
#17244=ADVANCED_FACE('',(#2285),#1403,.F.);
#17245=ADVANCED_FACE('',(#2286),#1404,.F.);
#17246=ADVANCED_FACE('',(#2287),#1405,.F.);
#17247=ADVANCED_FACE('',(#2288),#1406,.F.);
#17248=ADVANCED_FACE('',(#2289),#1407,.F.);
#17249=ADVANCED_FACE('',(#2290),#1408,.F.);
#17250=ADVANCED_FACE('',(#2291),#1409,.F.);
#17251=ADVANCED_FACE('',(#2292),#1410,.F.);
#17252=ADVANCED_FACE('',(#2293),#1411,.F.);
#17253=ADVANCED_FACE('',(#2294),#1412,.F.);
#17254=ADVANCED_FACE('',(#2295),#1413,.F.);
#17255=ADVANCED_FACE('',(#2296),#1414,.F.);
#17256=ADVANCED_FACE('',(#2297),#1415,.F.);
#17257=ADVANCED_FACE('',(#2298),#1416,.F.);
#17258=ADVANCED_FACE('',(#2299),#1417,.F.);
#17259=ADVANCED_FACE('',(#2300),#1418,.F.);
#17260=ADVANCED_FACE('',(#2301),#1419,.F.);
#17261=ADVANCED_FACE('',(#2302),#1420,.F.);
#17262=ADVANCED_FACE('',(#2303),#1421,.F.);
#17263=ADVANCED_FACE('',(#2304),#1422,.F.);
#17264=ADVANCED_FACE('',(#2305),#1423,.F.);
#17265=ADVANCED_FACE('',(#2306),#1424,.F.);
#17266=ADVANCED_FACE('',(#2307),#1425,.F.);
#17267=ADVANCED_FACE('',(#2308),#1426,.F.);
#17268=ADVANCED_FACE('',(#2309),#1427,.F.);
#17269=ADVANCED_FACE('',(#2310),#1428,.F.);
#17270=ADVANCED_FACE('',(#2311),#1429,.F.);
#17271=ADVANCED_FACE('',(#2312),#1430,.F.);
#17272=ADVANCED_FACE('',(#2313),#1431,.F.);
#17273=ADVANCED_FACE('',(#2314),#1432,.F.);
#17274=ADVANCED_FACE('',(#2315),#1433,.F.);
#17275=ADVANCED_FACE('',(#2316),#1434,.F.);
#17276=ADVANCED_FACE('',(#2317),#1435,.F.);
#17277=ADVANCED_FACE('',(#2318),#1436,.F.);
#17278=ADVANCED_FACE('',(#2319),#1437,.F.);
#17279=ADVANCED_FACE('',(#2320),#1438,.F.);
#17280=ADVANCED_FACE('',(#2321),#1439,.F.);
#17281=ADVANCED_FACE('',(#2322),#1440,.F.);
#17282=ADVANCED_FACE('',(#2323),#1441,.F.);
#17283=ADVANCED_FACE('',(#2324),#1442,.F.);
#17284=ADVANCED_FACE('',(#2325),#1443,.F.);
#17285=ADVANCED_FACE('',(#2326),#1444,.F.);
#17286=ADVANCED_FACE('',(#2327),#1445,.F.);
#17287=ADVANCED_FACE('',(#2328),#1446,.F.);
#17288=ADVANCED_FACE('',(#2329),#1447,.F.);
#17289=ADVANCED_FACE('',(#2330),#1448,.F.);
#17290=ADVANCED_FACE('',(#2331),#1449,.F.);
#17291=ADVANCED_FACE('',(#2332),#1450,.F.);
#17292=ADVANCED_FACE('',(#2333),#1451,.F.);
#17293=ADVANCED_FACE('',(#2334),#1452,.F.);
#17294=ADVANCED_FACE('',(#2335),#1453,.F.);
#17295=ADVANCED_FACE('',(#2336),#1454,.F.);
#17296=ADVANCED_FACE('',(#2337),#1455,.F.);
#17297=ADVANCED_FACE('',(#2338),#1456,.F.);
#17298=ADVANCED_FACE('',(#2339),#1457,.F.);
#17299=ADVANCED_FACE('',(#2340),#1458,.F.);
#17300=ADVANCED_FACE('',(#2341),#1459,.F.);
#17301=ADVANCED_FACE('',(#2342),#1460,.F.);
#17302=ADVANCED_FACE('',(#2343),#1461,.F.);
#17303=ADVANCED_FACE('',(#2344),#1462,.F.);
#17304=ADVANCED_FACE('',(#2345),#1463,.F.);
#17305=ADVANCED_FACE('',(#2346),#1464,.F.);
#17306=ADVANCED_FACE('',(#2347),#1465,.F.);
#17307=ADVANCED_FACE('',(#2348),#1466,.F.);
#17308=ADVANCED_FACE('',(#2349),#1467,.F.);
#17309=ADVANCED_FACE('',(#2350),#1468,.F.);
#17310=ADVANCED_FACE('',(#2351),#1469,.F.);
#17311=ADVANCED_FACE('',(#2352),#1470,.F.);
#17312=ADVANCED_FACE('',(#2353),#1471,.F.);
#17313=ADVANCED_FACE('',(#2354),#1472,.F.);
#17314=ADVANCED_FACE('',(#2355),#1473,.F.);
#17315=ADVANCED_FACE('',(#2356),#1474,.F.);
#17316=ADVANCED_FACE('',(#2357),#1475,.F.);
#17317=ADVANCED_FACE('',(#2358),#184,.T.);
#17318=ADVANCED_FACE('',(#2359),#1082,.T.);
#17319=ADVANCED_FACE('',(#2360),#16508,.T.);
#17320=ADVANCED_FACE('',(#2361),#1476,.T.);
#17321=ADVANCED_FACE('',(#2362),#1477,.T.);
#17322=ADVANCED_FACE('',(#2363),#1478,.T.);
#17323=ADVANCED_FACE('',(#2364,#904),#1479,.F.);
#17324=ADVANCED_FACE('',(#2365),#1480,.F.);
#17325=ADVANCED_FACE('',(#2366),#1481,.F.);
#17326=ADVANCED_FACE('',(#2367),#1482,.T.);
#17327=ADVANCED_FACE('',(#2368),#185,.F.);
#17328=ADVANCED_FACE('',(#2369),#1083,.T.);
#17329=ADVANCED_FACE('',(#2370),#1084,.T.);
#17330=ADVANCED_FACE('',(#2371),#1085,.T.);
#17331=ADVANCED_FACE('',(#2372),#16509,.T.);
#17332=ADVANCED_FACE('',(#2373),#1086,.T.);
#17333=ADVANCED_FACE('',(#2374),#1087,.T.);
#17334=ADVANCED_FACE('',(#2375),#16510,.T.);
#17335=ADVANCED_FACE('',(#2376),#1088,.T.);
#17336=ADVANCED_FACE('',(#2377),#1089,.T.);
#17337=ADVANCED_FACE('',(#2378),#16511,.T.);
#17338=ADVANCED_FACE('',(#2379),#1090,.T.);
#17339=ADVANCED_FACE('',(#2380),#1091,.T.);
#17340=ADVANCED_FACE('',(#2381),#16512,.T.);
#17341=ADVANCED_FACE('',(#2382),#1092,.T.);
#17342=ADVANCED_FACE('',(#2383),#1093,.T.);
#17343=ADVANCED_FACE('',(#2384),#16513,.T.);
#17344=ADVANCED_FACE('',(#2385),#1094,.T.);
#17345=ADVANCED_FACE('',(#2386),#1095,.T.);
#17346=ADVANCED_FACE('',(#2387),#16514,.T.);
#17347=ADVANCED_FACE('',(#2388),#1096,.T.);
#17348=ADVANCED_FACE('',(#2389),#1097,.T.);
#17349=ADVANCED_FACE('',(#2390),#16515,.T.);
#17350=ADVANCED_FACE('',(#2391),#1098,.T.);
#17351=ADVANCED_FACE('',(#2392),#1099,.T.);
#17352=ADVANCED_FACE('',(#2393),#16516,.T.);
#17353=ADVANCED_FACE('',(#2394),#1100,.T.);
#17354=ADVANCED_FACE('',(#2395),#1101,.T.);
#17355=ADVANCED_FACE('',(#2396),#16517,.T.);
#17356=ADVANCED_FACE('',(#2397),#1102,.T.);
#17357=ADVANCED_FACE('',(#2398),#1103,.T.);
#17358=ADVANCED_FACE('',(#2399),#16518,.T.);
#17359=ADVANCED_FACE('',(#2400),#1104,.T.);
#17360=ADVANCED_FACE('',(#2401),#1105,.T.);
#17361=ADVANCED_FACE('',(#2402),#16519,.T.);
#17362=ADVANCED_FACE('',(#2403),#1106,.T.);
#17363=ADVANCED_FACE('',(#2404),#1107,.T.);
#17364=ADVANCED_FACE('',(#2405),#16520,.T.);
#17365=ADVANCED_FACE('',(#2406),#1108,.T.);
#17366=ADVANCED_FACE('',(#2407),#1109,.T.);
#17367=ADVANCED_FACE('',(#2408),#16521,.T.);
#17368=ADVANCED_FACE('',(#2409),#1110,.T.);
#17369=ADVANCED_FACE('',(#2410),#1111,.T.);
#17370=ADVANCED_FACE('',(#2411),#16522,.T.);
#17371=ADVANCED_FACE('',(#2412),#16523,.T.);
#17372=ADVANCED_FACE('',(#2413),#16524,.T.);
#17373=ADVANCED_FACE('',(#2414),#16525,.T.);
#17374=ADVANCED_FACE('',(#2415),#16526,.T.);
#17375=ADVANCED_FACE('',(#2416),#16527,.T.);
#17376=ADVANCED_FACE('',(#2417),#16528,.T.);
#17377=ADVANCED_FACE('',(#2418),#16529,.T.);
#17378=ADVANCED_FACE('',(#2419),#16530,.T.);
#17379=ADVANCED_FACE('',(#2420),#16531,.T.);
#17380=ADVANCED_FACE('',(#2421),#16532,.T.);
#17381=ADVANCED_FACE('',(#2422),#16533,.T.);
#17382=ADVANCED_FACE('',(#2423),#16534,.T.);
#17383=ADVANCED_FACE('',(#2424),#16535,.T.);
#17384=ADVANCED_FACE('',(#2425),#16536,.T.);
#17385=ADVANCED_FACE('',(#2426),#16537,.T.);
#17386=ADVANCED_FACE('',(#2427),#16538,.T.);
#17387=ADVANCED_FACE('',(#2428),#16539,.T.);
#17388=ADVANCED_FACE('',(#2429),#16540,.T.);
#17389=ADVANCED_FACE('',(#2430),#16541,.T.);
#17390=ADVANCED_FACE('',(#2431),#16542,.T.);
#17391=ADVANCED_FACE('',(#2432),#16543,.T.);
#17392=ADVANCED_FACE('',(#2433),#16544,.T.);
#17393=ADVANCED_FACE('',(#2434),#16545,.T.);
#17394=ADVANCED_FACE('',(#2435),#16546,.T.);
#17395=ADVANCED_FACE('',(#2436),#16547,.T.);
#17396=ADVANCED_FACE('',(#2437),#16548,.T.);
#17397=ADVANCED_FACE('',(#2438),#16549,.T.);
#17398=ADVANCED_FACE('',(#2439),#16550,.T.);
#17399=ADVANCED_FACE('',(#2440),#16551,.T.);
#17400=ADVANCED_FACE('',(#2441),#16552,.T.);
#17401=ADVANCED_FACE('',(#2442),#16553,.T.);
#17402=ADVANCED_FACE('',(#2443),#16554,.T.);
#17403=ADVANCED_FACE('',(#2444),#16555,.T.);
#17404=ADVANCED_FACE('',(#2445),#16556,.T.);
#17405=ADVANCED_FACE('',(#2446),#16557,.T.);
#17406=ADVANCED_FACE('',(#2447),#16558,.T.);
#17407=ADVANCED_FACE('',(#2448),#16559,.T.);
#17408=ADVANCED_FACE('',(#2449),#16560,.T.);
#17409=ADVANCED_FACE('',(#2450),#16561,.T.);
#17410=ADVANCED_FACE('',(#2451),#16562,.T.);
#17411=ADVANCED_FACE('',(#2452),#16563,.T.);
#17412=ADVANCED_FACE('',(#2453),#16564,.T.);
#17413=ADVANCED_FACE('',(#2454),#16565,.T.);
#17414=ADVANCED_FACE('',(#2455),#16566,.T.);
#17415=ADVANCED_FACE('',(#2456),#16567,.T.);
#17416=ADVANCED_FACE('',(#2457),#16568,.T.);
#17417=ADVANCED_FACE('',(#2458),#16569,.T.);
#17418=ADVANCED_FACE('',(#2459),#16570,.T.);
#17419=ADVANCED_FACE('',(#2460),#16571,.T.);
#17420=ADVANCED_FACE('',(#2461),#16572,.T.);
#17421=ADVANCED_FACE('',(#2462),#16573,.T.);
#17422=ADVANCED_FACE('',(#2463),#16574,.T.);
#17423=ADVANCED_FACE('',(#2464),#16575,.T.);
#17424=ADVANCED_FACE('',(#2465),#16576,.T.);
#17425=ADVANCED_FACE('',(#2466),#16577,.T.);
#17426=ADVANCED_FACE('',(#2467),#16578,.T.);
#17427=ADVANCED_FACE('',(#2468),#16579,.T.);
#17428=ADVANCED_FACE('',(#2469),#16580,.T.);
#17429=ADVANCED_FACE('',(#2470),#16581,.T.);
#17430=ADVANCED_FACE('',(#2471),#16582,.T.);
#17431=ADVANCED_FACE('',(#2472),#16583,.T.);
#17432=ADVANCED_FACE('',(#2473),#16584,.T.);
#17433=ADVANCED_FACE('',(#2474),#16585,.T.);
#17434=ADVANCED_FACE('',(#2475),#16586,.T.);
#17435=ADVANCED_FACE('',(#2476),#16587,.T.);
#17436=ADVANCED_FACE('',(#2477),#16588,.T.);
#17437=ADVANCED_FACE('',(#2478),#16589,.T.);
#17438=ADVANCED_FACE('',(#2479),#16590,.T.);
#17439=ADVANCED_FACE('',(#2480),#16591,.T.);
#17440=ADVANCED_FACE('',(#2481),#16592,.T.);
#17441=ADVANCED_FACE('',(#2482),#16593,.T.);
#17442=ADVANCED_FACE('',(#2483),#16594,.T.);
#17443=ADVANCED_FACE('',(#2484),#16595,.T.);
#17444=ADVANCED_FACE('',(#2485),#16596,.T.);
#17445=ADVANCED_FACE('',(#2486),#16597,.T.);
#17446=ADVANCED_FACE('',(#2487),#16598,.T.);
#17447=ADVANCED_FACE('',(#2488),#1483,.T.);
#17448=ADVANCED_FACE('',(#2489),#16599,.T.);
#17449=ADVANCED_FACE('',(#2490,#905),#1484,.F.);
#17450=ADVANCED_FACE('',(#2491,#906),#1485,.T.);
#17451=ADVANCED_FACE('',(#2492),#1486,.T.);
#17452=ADVANCED_FACE('',(#2493),#1487,.F.);
#17453=ADVANCED_FACE('',(#2494),#1488,.F.);
#17454=ADVANCED_FACE('',(#2495),#1489,.F.);
#17455=ADVANCED_FACE('',(#2496),#1490,.F.);
#17456=ADVANCED_FACE('',(#2497),#1491,.F.);
#17457=ADVANCED_FACE('',(#2498),#1492,.F.);
#17458=ADVANCED_FACE('',(#2499),#1493,.F.);
#17459=ADVANCED_FACE('',(#2500),#1494,.F.);
#17460=ADVANCED_FACE('',(#2501),#1495,.F.);
#17461=ADVANCED_FACE('',(#2502),#1496,.F.);
#17462=ADVANCED_FACE('',(#2503),#1497,.F.);
#17463=ADVANCED_FACE('',(#2504),#1498,.F.);
#17464=ADVANCED_FACE('',(#2505),#1499,.F.);
#17465=ADVANCED_FACE('',(#2506),#1500,.F.);
#17466=ADVANCED_FACE('',(#2507),#1501,.F.);
#17467=ADVANCED_FACE('',(#2508),#1502,.F.);
#17468=ADVANCED_FACE('',(#2509),#1503,.F.);
#17469=ADVANCED_FACE('',(#2510),#1504,.F.);
#17470=ADVANCED_FACE('',(#2511),#1505,.F.);
#17471=ADVANCED_FACE('',(#2512),#1506,.F.);
#17472=ADVANCED_FACE('',(#2513),#1507,.F.);
#17473=ADVANCED_FACE('',(#2514),#1508,.F.);
#17474=ADVANCED_FACE('',(#2515),#1509,.F.);
#17475=ADVANCED_FACE('',(#2516),#1510,.F.);
#17476=ADVANCED_FACE('',(#2517),#1511,.F.);
#17477=ADVANCED_FACE('',(#2518),#1512,.F.);
#17478=ADVANCED_FACE('',(#2519),#1513,.F.);
#17479=ADVANCED_FACE('',(#2520),#1514,.F.);
#17480=ADVANCED_FACE('',(#2521),#1515,.F.);
#17481=ADVANCED_FACE('',(#2522),#1516,.F.);
#17482=ADVANCED_FACE('',(#2523),#1517,.F.);
#17483=ADVANCED_FACE('',(#2524),#1518,.F.);
#17484=ADVANCED_FACE('',(#2525),#1519,.F.);
#17485=ADVANCED_FACE('',(#2526),#1520,.F.);
#17486=ADVANCED_FACE('',(#2527),#1521,.F.);
#17487=ADVANCED_FACE('',(#2528),#1522,.F.);
#17488=ADVANCED_FACE('',(#2529),#1523,.F.);
#17489=ADVANCED_FACE('',(#2530),#1524,.F.);
#17490=ADVANCED_FACE('',(#2531),#1525,.F.);
#17491=ADVANCED_FACE('',(#2532),#1526,.F.);
#17492=ADVANCED_FACE('',(#2533),#1527,.F.);
#17493=ADVANCED_FACE('',(#2534),#1528,.F.);
#17494=ADVANCED_FACE('',(#2535),#1529,.F.);
#17495=ADVANCED_FACE('',(#2536),#1530,.F.);
#17496=ADVANCED_FACE('',(#2537),#1531,.F.);
#17497=ADVANCED_FACE('',(#2538),#1532,.F.);
#17498=ADVANCED_FACE('',(#2539),#1533,.F.);
#17499=ADVANCED_FACE('',(#2540),#1534,.F.);
#17500=ADVANCED_FACE('',(#2541),#1535,.F.);
#17501=ADVANCED_FACE('',(#2542),#1536,.F.);
#17502=ADVANCED_FACE('',(#2543),#1537,.F.);
#17503=ADVANCED_FACE('',(#2544),#1538,.F.);
#17504=ADVANCED_FACE('',(#2545),#1539,.F.);
#17505=ADVANCED_FACE('',(#2546),#1540,.F.);
#17506=ADVANCED_FACE('',(#2547),#1541,.F.);
#17507=ADVANCED_FACE('',(#2548),#1542,.F.);
#17508=ADVANCED_FACE('',(#2549),#1543,.F.);
#17509=ADVANCED_FACE('',(#2550),#1544,.F.);
#17510=ADVANCED_FACE('',(#2551),#1545,.F.);
#17511=ADVANCED_FACE('',(#2552),#1546,.F.);
#17512=ADVANCED_FACE('',(#2553),#1547,.F.);
#17513=ADVANCED_FACE('',(#2554),#1548,.F.);
#17514=ADVANCED_FACE('',(#2555),#1549,.F.);
#17515=ADVANCED_FACE('',(#2556),#1550,.F.);
#17516=ADVANCED_FACE('',(#2557),#1551,.F.);
#17517=ADVANCED_FACE('',(#2558),#1552,.F.);
#17518=ADVANCED_FACE('',(#2559),#1553,.F.);
#17519=ADVANCED_FACE('',(#2560),#1554,.F.);
#17520=ADVANCED_FACE('',(#2561),#1555,.F.);
#17521=ADVANCED_FACE('',(#2562),#1556,.F.);
#17522=ADVANCED_FACE('',(#2563),#1557,.F.);
#17523=ADVANCED_FACE('',(#2564),#1558,.F.);
#17524=ADVANCED_FACE('',(#2565),#1559,.F.);
#17525=ADVANCED_FACE('',(#2566),#1560,.F.);
#17526=ADVANCED_FACE('',(#2567),#1561,.F.);
#17527=ADVANCED_FACE('',(#2568),#1562,.F.);
#17528=ADVANCED_FACE('',(#2569),#1563,.F.);
#17529=ADVANCED_FACE('',(#2570),#1564,.F.);
#17530=ADVANCED_FACE('',(#2571),#1565,.F.);
#17531=ADVANCED_FACE('',(#2572),#1566,.F.);
#17532=ADVANCED_FACE('',(#2573),#1567,.F.);
#17533=ADVANCED_FACE('',(#2574),#1568,.F.);
#17534=ADVANCED_FACE('',(#2575),#1569,.F.);
#17535=ADVANCED_FACE('',(#2576),#1570,.F.);
#17536=ADVANCED_FACE('',(#2577),#1571,.F.);
#17537=ADVANCED_FACE('',(#2578),#1572,.F.);
#17538=ADVANCED_FACE('',(#2579),#1573,.F.);
#17539=ADVANCED_FACE('',(#2580),#1574,.F.);
#17540=ADVANCED_FACE('',(#2581),#1575,.F.);
#17541=ADVANCED_FACE('',(#2582),#1576,.F.);
#17542=ADVANCED_FACE('',(#2583),#1577,.F.);
#17543=ADVANCED_FACE('',(#2584),#1578,.F.);
#17544=ADVANCED_FACE('',(#2585),#1579,.F.);
#17545=ADVANCED_FACE('',(#2586),#1580,.F.);
#17546=ADVANCED_FACE('',(#2587),#1581,.F.);
#17547=ADVANCED_FACE('',(#2588),#1582,.F.);
#17548=ADVANCED_FACE('',(#2589),#1583,.F.);
#17549=ADVANCED_FACE('',(#2590),#1584,.F.);
#17550=ADVANCED_FACE('',(#2591),#1585,.F.);
#17551=ADVANCED_FACE('',(#2592),#1586,.F.);
#17552=ADVANCED_FACE('',(#2593),#1587,.F.);
#17553=ADVANCED_FACE('',(#2594),#1588,.F.);
#17554=ADVANCED_FACE('',(#2595),#1589,.F.);
#17555=ADVANCED_FACE('',(#2596),#1590,.F.);
#17556=ADVANCED_FACE('',(#2597),#1591,.F.);
#17557=ADVANCED_FACE('',(#2598),#1592,.F.);
#17558=ADVANCED_FACE('',(#2599),#1593,.F.);
#17559=ADVANCED_FACE('',(#2600),#1594,.F.);
#17560=ADVANCED_FACE('',(#2601),#1595,.F.);
#17561=ADVANCED_FACE('',(#2602),#1596,.F.);
#17562=ADVANCED_FACE('',(#2603),#1597,.F.);
#17563=ADVANCED_FACE('',(#2604),#1598,.F.);
#17564=ADVANCED_FACE('',(#2605),#1599,.F.);
#17565=ADVANCED_FACE('',(#2606),#1600,.F.);
#17566=ADVANCED_FACE('',(#2607),#1601,.F.);
#17567=ADVANCED_FACE('',(#2608),#1602,.F.);
#17568=ADVANCED_FACE('',(#2609),#1603,.F.);
#17569=ADVANCED_FACE('',(#2610),#1604,.F.);
#17570=ADVANCED_FACE('',(#2611),#1605,.F.);
#17571=ADVANCED_FACE('',(#2612),#1606,.F.);
#17572=ADVANCED_FACE('',(#2613),#1607,.F.);
#17573=ADVANCED_FACE('',(#2614),#1608,.F.);
#17574=ADVANCED_FACE('',(#2615),#1609,.F.);
#17575=ADVANCED_FACE('',(#2616),#1610,.F.);
#17576=ADVANCED_FACE('',(#2617),#1611,.F.);
#17577=ADVANCED_FACE('',(#2618),#1612,.F.);
#17578=ADVANCED_FACE('',(#2619),#1613,.F.);
#17579=ADVANCED_FACE('',(#2620),#1614,.F.);
#17580=ADVANCED_FACE('',(#2621),#1615,.F.);
#17581=ADVANCED_FACE('',(#2622),#1616,.F.);
#17582=ADVANCED_FACE('',(#2623),#1617,.F.);
#17583=ADVANCED_FACE('',(#2624),#1618,.F.);
#17584=ADVANCED_FACE('',(#2625),#1619,.F.);
#17585=ADVANCED_FACE('',(#2626),#1620,.F.);
#17586=ADVANCED_FACE('',(#2627),#1621,.F.);
#17587=ADVANCED_FACE('',(#2628),#1622,.F.);
#17588=ADVANCED_FACE('',(#2629),#1623,.F.);
#17589=ADVANCED_FACE('',(#2630),#1624,.F.);
#17590=ADVANCED_FACE('',(#2631),#1625,.F.);
#17591=ADVANCED_FACE('',(#2632),#1626,.F.);
#17592=ADVANCED_FACE('',(#2633),#1627,.F.);
#17593=ADVANCED_FACE('',(#2634),#1628,.F.);
#17594=ADVANCED_FACE('',(#2635),#1629,.F.);
#17595=ADVANCED_FACE('',(#2636),#1630,.F.);
#17596=ADVANCED_FACE('',(#2637),#1631,.F.);
#17597=ADVANCED_FACE('',(#2638),#1632,.F.);
#17598=ADVANCED_FACE('',(#2639),#1633,.F.);
#17599=ADVANCED_FACE('',(#2640),#1634,.F.);
#17600=ADVANCED_FACE('',(#2641),#1635,.F.);
#17601=ADVANCED_FACE('',(#2642),#1636,.F.);
#17602=ADVANCED_FACE('',(#2643),#1637,.F.);
#17603=ADVANCED_FACE('',(#2644),#1638,.F.);
#17604=ADVANCED_FACE('',(#2645),#1639,.F.);
#17605=ADVANCED_FACE('',(#2646),#1640,.F.);
#17606=CLOSED_SHELL('',(#16600,#16601,#16602,#16603,#16604,#16605,#16606,
#16607,#16608,#16609));
#17607=CLOSED_SHELL('',(#16610,#16611,#16612,#16613,#16614,#16615,#16616,
#16617,#16618,#16619));
#17608=CLOSED_SHELL('',(#16620,#16621,#16622,#16623,#16624,#16625,#16626,
#16627,#16628,#16629));
#17609=CLOSED_SHELL('',(#16630,#16631,#16632,#16633,#16634,#16635,#16636,
#16637,#16638,#16639));
#17610=CLOSED_SHELL('',(#16640,#16641,#16642,#16643,#16644,#16645));
#17611=CLOSED_SHELL('',(#16646,#16647,#16648,#16649,#16650,#16651));
#17612=CLOSED_SHELL('',(#16652,#16653,#16654,#16655,#16656,#16657,#16658,
#16659,#16660,#16661));
#17613=CLOSED_SHELL('',(#16662,#16663,#16664,#16665,#16666,#16667,#16668,
#16669,#16670));
#17614=CLOSED_SHELL('',(#16671,#16672,#16673,#16674,#16675,#16676,#16677,
#16678,#16679,#16680,#16681,#16682,#16683,#16684,#16685,#16686,#16687,#16688,
#16689,#16690,#16691,#16692,#16693,#16694,#16695,#16696,#16697,#16698,#16699,
#16700,#16701,#16702,#16703,#16704,#16705,#16706,#16707,#16708,#16709,#16710,
#16711,#16712,#16713,#16714,#16715,#16716,#16717,#16718,#16719,#16720,#16721,
#16722,#16723,#16724,#16725,#16726,#16727,#16728,#16729,#16730,#16731,#16732,
#16733,#16734,#16735,#16736,#16737,#16738,#16739,#16740,#16741));
#17615=CLOSED_SHELL('',(#16742,#16743,#16744,#16745,#16746));
#17616=CLOSED_SHELL('',(#16747,#16748,#16749,#16750));
#17617=CLOSED_SHELL('',(#16751,#16752,#16753,#16754,#16755,#16756));
#17618=CLOSED_SHELL('',(#16757,#16758,#16759,#16760,#16761,#16762,#16763,
#16764,#16765,#16766));
#17619=CLOSED_SHELL('',(#16767,#16768,#16769,#16770,#16771,#16772,#16773,
#16774,#16775,#16776,#16777,#16778,#16779,#16780,#16781,#16782,#16783,#16784,
#16785,#16786,#16787,#16788,#16789,#16790,#16791,#16792,#16793,#16794,#16795,
#16796,#16797,#16798,#16799,#16800,#16801));
#17620=CLOSED_SHELL('',(#16802,#16803,#16804,#16805,#16806,#16807,#16808,
#16809,#16810));
#17621=CLOSED_SHELL('',(#16811,#16812,#16813,#16814,#16815,#16816,#16817,
#16818,#16819,#16820,#16821,#16822,#16823,#16824,#16825,#16826,#16827,#16828,
#16829));
#17622=CLOSED_SHELL('',(#16830,#16831,#16832,#16833,#16834,#16835,#16836,
#16837,#16838));
#17623=CLOSED_SHELL('',(#16839,#16840,#16841,#16842,#16843,#16844,#16845,
#16846,#16847,#16848,#16849));
#17624=CLOSED_SHELL('',(#16850,#16851,#16852,#16853,#16854,#16855,#16856,
#16857,#16858,#16859,#16860,#16861,#16862,#16863,#16864,#16865,#16866,#16867,
#16868,#16869,#16870,#16871,#16872,#16873,#16874,#16875,#16876,#16877,#16878,
#16879,#16880,#16881,#16882,#16883,#16884,#16885,#16886,#16887,#16888,#16889,
#16890,#16891,#16892,#16893,#16894,#16895,#16896,#16897,#16898,#16899,#16900,
#16901,#16902,#16903,#16904,#16905,#16906,#16907,#16908,#16909,#16910,#16911,
#16912,#16913,#16914,#16915,#16916,#16917,#16918,#16919,#16920,#16921,#16922,
#16923,#16924,#16925,#16926,#16927));
#17625=CLOSED_SHELL('',(#16928,#16929,#16930,#16931,#16932,#16933,#16934,
#16935,#16936,#16937,#16938,#16939,#16940,#16941,#16942,#16943,#16944,#16945,
#16946,#16947,#16948,#16949,#16950,#16951,#16952,#16953,#16954,#16955,#16956,
#16957,#16958,#16959,#16960,#16961,#16962,#16963,#16964,#16965,#16966,#16967,
#16968,#16969,#16970,#16971,#16972,#16973,#16974,#16975,#16976,#16977,#16978,
#16979,#16980,#16981,#16982,#16983,#16984,#16985,#16986,#16987,#16988,#16989,
#16990,#16991,#16992,#16993,#16994,#16995,#16996,#16997,#16998,#16999,#17000,
#17001,#17002,#17003));
#17626=CLOSED_SHELL('',(#17004,#17005,#17006,#17007,#17008));
#17627=CLOSED_SHELL('',(#17009,#17010,#17011,#17012,#17013,#17014,#17015,
#17016,#17017,#17018,#17019,#17020,#17021,#17022,#17023,#17024,#17025,#17026,
#17027,#17028,#17029,#17030));
#17628=CLOSED_SHELL('',(#17031,#17032,#17033));
#17629=CLOSED_SHELL('',(#17034,#17035,#17036,#17037,#17038,#17039,#17040,
#17041,#17042,#17043,#17044,#17045,#17046,#17047,#17048,#17049,#17050,#17051,
#17052,#17053,#17054,#17055,#17056,#17057,#17058,#17059,#17060,#17061,#17062,
#17063,#17064,#17065,#17066,#17067,#17068,#17069,#17070,#17071,#17072,#17073,
#17074,#17075,#17076,#17077,#17078,#17079,#17080,#17081,#17082,#17083,#17084,
#17085,#17086,#17087,#17088,#17089,#17090,#17091,#17092,#17093,#17094,#17095,
#17096,#17097,#17098,#17099,#17100,#17101,#17102,#17103,#17104,#17105,#17106,
#17107,#17108,#17109,#17110,#17111,#17112,#17113,#17114,#17115,#17116,#17117,
#17118,#17119,#17120,#17121,#17122,#17123,#17124,#17125,#17126,#17127,#17128,
#17129,#17130,#17131,#17132,#17133,#17134,#17135,#17136,#17137,#17138,#17139,
#17140,#17141,#17142,#17143,#17144,#17145,#17146,#17147,#17148,#17149,#17150,
#17151,#17152,#17153,#17154,#17155,#17156,#17157,#17158,#17159,#17160,#17161,
#17162,#17163,#17164,#17165,#17166,#17167,#17168,#17169,#17170,#17171,#17172,
#17173,#17174,#17175,#17176,#17177,#17178,#17179,#17180,#17181,#17182,#17183,
#17184,#17185,#17186,#17187,#17188,#17189,#17190,#17191,#17192,#17193,#17194,
#17195,#17196,#17197,#17198,#17199,#17200,#17201,#17202,#17203,#17204,#17205,
#17206,#17207,#17208,#17209,#17210,#17211,#17212,#17213,#17214,#17215,#17216,
#17217,#17218,#17219,#17220,#17221,#17222,#17223,#17224,#17225,#17226,#17227,
#17228,#17229,#17230,#17231,#17232,#17233,#17234,#17235,#17236,#17237,#17238,
#17239,#17240,#17241,#17242,#17243,#17244,#17245,#17246,#17247,#17248,#17249,
#17250,#17251,#17252,#17253,#17254,#17255,#17256,#17257,#17258,#17259,#17260,
#17261,#17262,#17263,#17264,#17265,#17266,#17267,#17268,#17269,#17270,#17271,
#17272,#17273,#17274,#17275,#17276,#17277,#17278,#17279,#17280,#17281,#17282,
#17283,#17284,#17285,#17286,#17287,#17288,#17289,#17290,#17291,#17292,#17293,
#17294,#17295,#17296,#17297,#17298,#17299,#17300,#17301,#17302,#17303,#17304,
#17305,#17306,#17307,#17308,#17309,#17310,#17311,#17312,#17313,#17314,#17315,
#17316));
#17630=CLOSED_SHELL('',(#17317,#17318,#17319,#17320,#17321,#17322,#17323,
#17324,#17325,#17326));
#17631=CLOSED_SHELL('',(#17327,#17328,#17329,#17330,#17331,#17332,#17333,
#17334,#17335,#17336,#17337,#17338,#17339,#17340,#17341,#17342,#17343,#17344,
#17345,#17346,#17347,#17348,#17349,#17350,#17351,#17352,#17353,#17354,#17355,
#17356,#17357,#17358,#17359,#17360,#17361,#17362,#17363,#17364,#17365,#17366,
#17367,#17368,#17369,#17370,#17371,#17372,#17373,#17374,#17375,#17376,#17377,
#17378,#17379,#17380,#17381,#17382,#17383,#17384,#17385,#17386,#17387,#17388,
#17389,#17390,#17391,#17392,#17393,#17394,#17395,#17396,#17397,#17398,#17399,
#17400,#17401,#17402,#17403,#17404,#17405,#17406,#17407,#17408,#17409,#17410,
#17411,#17412,#17413,#17414,#17415,#17416,#17417,#17418,#17419,#17420,#17421,
#17422,#17423,#17424,#17425,#17426,#17427,#17428,#17429,#17430,#17431,#17432,
#17433,#17434,#17435,#17436,#17437,#17438,#17439,#17440,#17441,#17442,#17443,
#17444,#17445,#17446,#17447,#17448,#17449,#17450,#17451,#17452,#17453,#17454,
#17455,#17456,#17457,#17458,#17459,#17460,#17461,#17462,#17463,#17464,#17465,
#17466,#17467,#17468,#17469,#17470,#17471,#17472,#17473,#17474,#17475,#17476,
#17477,#17478,#17479,#17480,#17481,#17482,#17483,#17484,#17485,#17486,#17487,
#17488,#17489,#17490,#17491,#17492,#17493,#17494,#17495,#17496,#17497,#17498,
#17499,#17500,#17501,#17502,#17503,#17504,#17505,#17506,#17507,#17508,#17509,
#17510,#17511,#17512,#17513,#17514,#17515,#17516,#17517,#17518,#17519,#17520,
#17521,#17522,#17523,#17524,#17525,#17526,#17527,#17528,#17529,#17530,#17531,
#17532,#17533,#17534,#17535,#17536,#17537,#17538,#17539,#17540,#17541,#17542,
#17543,#17544,#17545,#17546,#17547,#17548,#17549,#17550,#17551,#17552,#17553,
#17554,#17555,#17556,#17557,#17558,#17559,#17560,#17561,#17562,#17563,#17564,
#17565,#17566,#17567,#17568,#17569,#17570,#17571,#17572,#17573,#17574,#17575,
#17576,#17577,#17578,#17579,#17580,#17581,#17582,#17583,#17584,#17585,#17586,
#17587,#17588,#17589,#17590,#17591,#17592,#17593,#17594,#17595,#17596,#17597,
#17598,#17599,#17600,#17601,#17602,#17603,#17604,#17605));
#17632=DERIVED_UNIT_ELEMENT(#17660,1.);
#17633=DERIVED_UNIT_ELEMENT(#38637,-3.);
#17634=DERIVED_UNIT_ELEMENT(#17660,1.);
#17635=DERIVED_UNIT_ELEMENT(#38637,-3.);
#17636=DERIVED_UNIT_ELEMENT(#17660,1.);
#17637=DERIVED_UNIT_ELEMENT(#38637,-3.);
#17638=DERIVED_UNIT_ELEMENT(#17660,1.);
#17639=DERIVED_UNIT_ELEMENT(#38637,-3.);
#17640=DERIVED_UNIT_ELEMENT(#17660,1.);
#17641=DERIVED_UNIT_ELEMENT(#38637,-3.);
#17642=DERIVED_UNIT_ELEMENT(#17660,1.);
#17643=DERIVED_UNIT_ELEMENT(#38637,-3.);
#17644=DERIVED_UNIT_ELEMENT(#17660,1.);
#17645=DERIVED_UNIT_ELEMENT(#38637,-3.);
#17646=DERIVED_UNIT_ELEMENT(#17660,1.);
#17647=DERIVED_UNIT_ELEMENT(#38637,-3.);
#17648=DERIVED_UNIT_ELEMENT(#17660,1.);
#17649=DERIVED_UNIT_ELEMENT(#38637,-3.);
#17650=DERIVED_UNIT_ELEMENT(#17660,1.);
#17651=DERIVED_UNIT_ELEMENT(#38637,-3.);
#17652=DERIVED_UNIT_ELEMENT(#17660,1.);
#17653=DERIVED_UNIT_ELEMENT(#38637,-3.);
#17654=DERIVED_UNIT_ELEMENT(#17660,1.);
#17655=DERIVED_UNIT_ELEMENT(#38637,-3.);
#17656=DERIVED_UNIT_ELEMENT(#17660,1.);
#17657=DERIVED_UNIT_ELEMENT(#38637,-3.);
#17658=DERIVED_UNIT_ELEMENT(#17660,1.);
#17659=DERIVED_UNIT_ELEMENT(#38637,-3.);
#17660=(
MASS_UNIT()
NAMED_UNIT(*)
SI_UNIT(.KILO.,.GRAM.)
);
#17661=DERIVED_UNIT((#17632,#17633));
#17662=DERIVED_UNIT((#17634,#17635));
#17663=DERIVED_UNIT((#17636,#17637));
#17664=DERIVED_UNIT((#17638,#17639));
#17665=DERIVED_UNIT((#17640,#17641));
#17666=DERIVED_UNIT((#17642,#17643));
#17667=DERIVED_UNIT((#17644,#17645));
#17668=DERIVED_UNIT((#17646,#17647));
#17669=DERIVED_UNIT((#17648,#17649));
#17670=DERIVED_UNIT((#17650,#17651));
#17671=DERIVED_UNIT((#17652,#17653));
#17672=DERIVED_UNIT((#17654,#17655));
#17673=DERIVED_UNIT((#17656,#17657));
#17674=DERIVED_UNIT((#17658,#17659));
#17675=MEASURE_REPRESENTATION_ITEM('density measure',
POSITIVE_RATIO_MEASURE(7850.),#17661);
#17676=MEASURE_REPRESENTATION_ITEM('density measure',
POSITIVE_RATIO_MEASURE(7850.),#17662);
#17677=MEASURE_REPRESENTATION_ITEM('density measure',
POSITIVE_RATIO_MEASURE(7850.),#17663);
#17678=MEASURE_REPRESENTATION_ITEM('density measure',
POSITIVE_RATIO_MEASURE(7850.),#17664);
#17679=MEASURE_REPRESENTATION_ITEM('density measure',
POSITIVE_RATIO_MEASURE(7850.),#17665);
#17680=MEASURE_REPRESENTATION_ITEM('density measure',
POSITIVE_RATIO_MEASURE(7850.),#17666);
#17681=MEASURE_REPRESENTATION_ITEM('density measure',
POSITIVE_RATIO_MEASURE(7850.),#17667);
#17682=MEASURE_REPRESENTATION_ITEM('density measure',
POSITIVE_RATIO_MEASURE(7850.),#17668);
#17683=MEASURE_REPRESENTATION_ITEM('density measure',
POSITIVE_RATIO_MEASURE(7850.),#17669);
#17684=MEASURE_REPRESENTATION_ITEM('density measure',
POSITIVE_RATIO_MEASURE(7850.),#17670);
#17685=MEASURE_REPRESENTATION_ITEM('density measure',
POSITIVE_RATIO_MEASURE(7850.),#17671);
#17686=MEASURE_REPRESENTATION_ITEM('density measure',
POSITIVE_RATIO_MEASURE(7850.),#17672);
#17687=MEASURE_REPRESENTATION_ITEM('density measure',
POSITIVE_RATIO_MEASURE(7850.),#17673);
#17688=MEASURE_REPRESENTATION_ITEM('density measure',
POSITIVE_RATIO_MEASURE(7850.),#17674);
#17689=PROPERTY_DEFINITION_REPRESENTATION(#17759,#17717);
#17690=PROPERTY_DEFINITION_REPRESENTATION(#17760,#17718);
#17691=PROPERTY_DEFINITION_REPRESENTATION(#17761,#17719);
#17692=PROPERTY_DEFINITION_REPRESENTATION(#17762,#17720);
#17693=PROPERTY_DEFINITION_REPRESENTATION(#17763,#17721);
#17694=PROPERTY_DEFINITION_REPRESENTATION(#17764,#17722);
#17695=PROPERTY_DEFINITION_REPRESENTATION(#17765,#17723);
#17696=PROPERTY_DEFINITION_REPRESENTATION(#17766,#17724);
#17697=PROPERTY_DEFINITION_REPRESENTATION(#17767,#17725);
#17698=PROPERTY_DEFINITION_REPRESENTATION(#17768,#17726);
#17699=PROPERTY_DEFINITION_REPRESENTATION(#17769,#17727);
#17700=PROPERTY_DEFINITION_REPRESENTATION(#17770,#17728);
#17701=PROPERTY_DEFINITION_REPRESENTATION(#17771,#17729);
#17702=PROPERTY_DEFINITION_REPRESENTATION(#17772,#17730);
#17703=PROPERTY_DEFINITION_REPRESENTATION(#17773,#17731);
#17704=PROPERTY_DEFINITION_REPRESENTATION(#17774,#17732);
#17705=PROPERTY_DEFINITION_REPRESENTATION(#17775,#17733);
#17706=PROPERTY_DEFINITION_REPRESENTATION(#17776,#17734);
#17707=PROPERTY_DEFINITION_REPRESENTATION(#17777,#17735);
#17708=PROPERTY_DEFINITION_REPRESENTATION(#17778,#17736);
#17709=PROPERTY_DEFINITION_REPRESENTATION(#17779,#17737);
#17710=PROPERTY_DEFINITION_REPRESENTATION(#17780,#17738);
#17711=PROPERTY_DEFINITION_REPRESENTATION(#17781,#17739);
#17712=PROPERTY_DEFINITION_REPRESENTATION(#17782,#17740);
#17713=PROPERTY_DEFINITION_REPRESENTATION(#17783,#17741);
#17714=PROPERTY_DEFINITION_REPRESENTATION(#17784,#17742);
#17715=PROPERTY_DEFINITION_REPRESENTATION(#17785,#17743);
#17716=PROPERTY_DEFINITION_REPRESENTATION(#17786,#17744);
#17717=REPRESENTATION('material name',(#17745),#38621);
#17718=REPRESENTATION('density',(#17675),#38621);
#17719=REPRESENTATION('material name',(#17746),#38622);
#17720=REPRESENTATION('density',(#17676),#38622);
#17721=REPRESENTATION('material name',(#17747),#38623);
#17722=REPRESENTATION('density',(#17677),#38623);
#17723=REPRESENTATION('material name',(#17748),#38624);
#17724=REPRESENTATION('density',(#17678),#38624);
#17725=REPRESENTATION('material name',(#17749),#38625);
#17726=REPRESENTATION('density',(#17679),#38625);
#17727=REPRESENTATION('material name',(#17750),#38626);
#17728=REPRESENTATION('density',(#17680),#38626);
#17729=REPRESENTATION('material name',(#17751),#38627);
#17730=REPRESENTATION('density',(#17681),#38627);
#17731=REPRESENTATION('material name',(#17752),#38628);
#17732=REPRESENTATION('density',(#17682),#38628);
#17733=REPRESENTATION('material name',(#17753),#38629);
#17734=REPRESENTATION('density',(#17683),#38629);
#17735=REPRESENTATION('material name',(#17754),#38630);
#17736=REPRESENTATION('density',(#17684),#38630);
#17737=REPRESENTATION('material name',(#17755),#38631);
#17738=REPRESENTATION('density',(#17685),#38631);
#17739=REPRESENTATION('material name',(#17756),#38632);
#17740=REPRESENTATION('density',(#17686),#38632);
#17741=REPRESENTATION('material name',(#17757),#38633);
#17742=REPRESENTATION('density',(#17687),#38633);
#17743=REPRESENTATION('material name',(#17758),#38634);
#17744=REPRESENTATION('density',(#17688),#38634);
#17745=DESCRIPTIVE_REPRESENTATION_ITEM('Steel','Steel');
#17746=DESCRIPTIVE_REPRESENTATION_ITEM('Steel','Steel');
#17747=DESCRIPTIVE_REPRESENTATION_ITEM('Steel','Steel');
#17748=DESCRIPTIVE_REPRESENTATION_ITEM('Steel','Steel');
#17749=DESCRIPTIVE_REPRESENTATION_ITEM('Steel','Steel');
#17750=DESCRIPTIVE_REPRESENTATION_ITEM('Steel','Steel');
#17751=DESCRIPTIVE_REPRESENTATION_ITEM('Steel','Steel');
#17752=DESCRIPTIVE_REPRESENTATION_ITEM('Steel','Steel');
#17753=DESCRIPTIVE_REPRESENTATION_ITEM('Steel','Steel');
#17754=DESCRIPTIVE_REPRESENTATION_ITEM('Steel','Steel');
#17755=DESCRIPTIVE_REPRESENTATION_ITEM('Steel','Steel');
#17756=DESCRIPTIVE_REPRESENTATION_ITEM('Steel','Steel');
#17757=DESCRIPTIVE_REPRESENTATION_ITEM('Steel','Steel');
#17758=DESCRIPTIVE_REPRESENTATION_ITEM('Steel','Steel');
#17759=PROPERTY_DEFINITION('material property','material name',#38701);
#17760=PROPERTY_DEFINITION('material property','density of part',#38701);
#17761=PROPERTY_DEFINITION('material property','material name',#38702);
#17762=PROPERTY_DEFINITION('material property','density of part',#38702);
#17763=PROPERTY_DEFINITION('material property','material name',#38703);
#17764=PROPERTY_DEFINITION('material property','density of part',#38703);
#17765=PROPERTY_DEFINITION('material property','material name',#38704);
#17766=PROPERTY_DEFINITION('material property','density of part',#38704);
#17767=PROPERTY_DEFINITION('material property','material name',#38705);
#17768=PROPERTY_DEFINITION('material property','density of part',#38705);
#17769=PROPERTY_DEFINITION('material property','material name',#38706);
#17770=PROPERTY_DEFINITION('material property','density of part',#38706);
#17771=PROPERTY_DEFINITION('material property','material name',#38707);
#17772=PROPERTY_DEFINITION('material property','density of part',#38707);
#17773=PROPERTY_DEFINITION('material property','material name',#38708);
#17774=PROPERTY_DEFINITION('material property','density of part',#38708);
#17775=PROPERTY_DEFINITION('material property','material name',#38709);
#17776=PROPERTY_DEFINITION('material property','density of part',#38709);
#17777=PROPERTY_DEFINITION('material property','material name',#38710);
#17778=PROPERTY_DEFINITION('material property','density of part',#38710);
#17779=PROPERTY_DEFINITION('material property','material name',#38711);
#17780=PROPERTY_DEFINITION('material property','density of part',#38711);
#17781=PROPERTY_DEFINITION('material property','material name',#38712);
#17782=PROPERTY_DEFINITION('material property','density of part',#38712);
#17783=PROPERTY_DEFINITION('material property','material name',#38713);
#17784=PROPERTY_DEFINITION('material property','density of part',#38713);
#17785=PROPERTY_DEFINITION('material property','material name',#38714);
#17786=PROPERTY_DEFINITION('material property','density of part',#38714);
#17787=AXIS2_PLACEMENT_3D('',#24599,#19743,#19744);
#17788=AXIS2_PLACEMENT_3D('',#24600,#19745,#19746);
#17789=AXIS2_PLACEMENT_3D('',#24601,#19747,#19748);
#17790=AXIS2_PLACEMENT_3D('',#24604,#19749,#19750);
#17791=AXIS2_PLACEMENT_3D('',#24608,#19752,#19753);
#17792=AXIS2_PLACEMENT_3D('',#24610,#19755,#19756);
#17793=AXIS2_PLACEMENT_3D('',#24613,#19757,#19758);
#17794=AXIS2_PLACEMENT_3D('',#24617,#19760,#19761);
#17795=AXIS2_PLACEMENT_3D('',#24619,#19763,#19764);
#17796=AXIS2_PLACEMENT_3D('',#24630,#19771,#19772);
#17797=AXIS2_PLACEMENT_3D('',#24641,#19779,#19780);
#17798=AXIS2_PLACEMENT_3D('',#24642,#19781,#19782);
#17799=AXIS2_PLACEMENT_3D('',#24643,#19783,#19784);
#17800=AXIS2_PLACEMENT_3D('',#24644,#19785,#19786);
#17801=AXIS2_PLACEMENT_3D('',#24645,#19787,#19788);
#17802=AXIS2_PLACEMENT_3D('',#24646,#19789,#19790);
#17803=AXIS2_PLACEMENT_3D('',#24647,#19791,#19792);
#17804=AXIS2_PLACEMENT_3D('',#24648,#19793,#19794);
#17805=AXIS2_PLACEMENT_3D('',#24649,#19795,#19796);
#17806=AXIS2_PLACEMENT_3D('',#24650,#19797,#19798);
#17807=AXIS2_PLACEMENT_3D('',#24651,#19799,#19800);
#17808=AXIS2_PLACEMENT_3D('',#24654,#19801,#19802);
#17809=AXIS2_PLACEMENT_3D('',#24658,#19804,#19805);
#17810=AXIS2_PLACEMENT_3D('',#24660,#19807,#19808);
#17811=AXIS2_PLACEMENT_3D('',#24663,#19809,#19810);
#17812=AXIS2_PLACEMENT_3D('',#24667,#19812,#19813);
#17813=AXIS2_PLACEMENT_3D('',#24669,#19815,#19816);
#17814=AXIS2_PLACEMENT_3D('',#24672,#19817,#19818);
#17815=AXIS2_PLACEMENT_3D('',#24676,#19820,#19821);
#17816=AXIS2_PLACEMENT_3D('',#24678,#19823,#19824);
#17817=AXIS2_PLACEMENT_3D('',#24686,#19830,#19831);
#17818=AXIS2_PLACEMENT_3D('',#24694,#19837,#19838);
#17819=AXIS2_PLACEMENT_3D('',#24695,#19839,#19840);
#17820=AXIS2_PLACEMENT_3D('',#24696,#19841,#19842);
#17821=AXIS2_PLACEMENT_3D('',#24697,#19843,#19844);
#17822=AXIS2_PLACEMENT_3D('',#24698,#19845,#19846);
#17823=AXIS2_PLACEMENT_3D('',#24699,#19847,#19848);
#17824=AXIS2_PLACEMENT_3D('',#24700,#19849,#19850);
#17825=AXIS2_PLACEMENT_3D('',#24701,#19851,#19852);
#17826=AXIS2_PLACEMENT_3D('',#24710,#19857,#19858);
#17827=AXIS2_PLACEMENT_3D('',#24724,#19866,#19867);
#17828=AXIS2_PLACEMENT_3D('',#24738,#19875,#19876);
#17829=AXIS2_PLACEMENT_3D('',#24739,#19877,#19878);
#17830=AXIS2_PLACEMENT_3D('',#24740,#19879,#19880);
#17831=AXIS2_PLACEMENT_3D('',#24741,#19881,#19882);
#17832=AXIS2_PLACEMENT_3D('',#24742,#19883,#19884);
#17833=AXIS2_PLACEMENT_3D('',#24743,#19885,#19886);
#17834=AXIS2_PLACEMENT_3D('',#24744,#19887,#19888);
#17835=AXIS2_PLACEMENT_3D('',#24745,#19889,#19890);
#17836=AXIS2_PLACEMENT_3D('',#24746,#19891,#19892);
#17837=AXIS2_PLACEMENT_3D('',#24747,#19893,#19894);
#17838=AXIS2_PLACEMENT_3D('',#24748,#19895,#19896);
#17839=AXIS2_PLACEMENT_3D('',#24749,#19897,#19898);
#17840=AXIS2_PLACEMENT_3D('',#24750,#19899,#19900);
#17841=AXIS2_PLACEMENT_3D('',#24751,#19901,#19902);
#17842=AXIS2_PLACEMENT_3D('',#24760,#19907,#19908);
#17843=AXIS2_PLACEMENT_3D('',#24774,#19916,#19917);
#17844=AXIS2_PLACEMENT_3D('',#24788,#19925,#19926);
#17845=AXIS2_PLACEMENT_3D('',#24789,#19927,#19928);
#17846=AXIS2_PLACEMENT_3D('',#24790,#19929,#19930);
#17847=AXIS2_PLACEMENT_3D('',#24791,#19931,#19932);
#17848=AXIS2_PLACEMENT_3D('',#24792,#19933,#19934);
#17849=AXIS2_PLACEMENT_3D('',#24793,#19935,#19936);
#17850=AXIS2_PLACEMENT_3D('',#24794,#19937,#19938);
#17851=AXIS2_PLACEMENT_3D('',#24795,#19939,#19940);
#17852=AXIS2_PLACEMENT_3D('',#24796,#19941,#19942);
#17853=AXIS2_PLACEMENT_3D('',#24797,#19943,#19944);
#17854=AXIS2_PLACEMENT_3D('',#24798,#19945,#19946);
#17855=AXIS2_PLACEMENT_3D('',#24799,#19947,#19948);
#17856=AXIS2_PLACEMENT_3D('',#24800,#19949,#19950);
#17857=AXIS2_PLACEMENT_3D('',#24801,#19951,#19952);
#17858=AXIS2_PLACEMENT_3D('',#24802,#19953,#19954);
#17859=AXIS2_PLACEMENT_3D('',#24805,#19955,#19956);
#17860=AXIS2_PLACEMENT_3D('',#24809,#19958,#19959);
#17861=AXIS2_PLACEMENT_3D('',#24811,#19961,#19962);
#17862=AXIS2_PLACEMENT_3D('',#24814,#19963,#19964);
#17863=AXIS2_PLACEMENT_3D('',#24816,#19966,#19967);
#17864=AXIS2_PLACEMENT_3D('',#24824,#19973,#19974);
#17865=AXIS2_PLACEMENT_3D('',#24825,#19975,#19976);
#17866=AXIS2_PLACEMENT_3D('',#24826,#19977,#19978);
#17867=AXIS2_PLACEMENT_3D('',#24827,#19979,#19980);
#17868=AXIS2_PLACEMENT_3D('',#24828,#19981,#19982);
#17869=AXIS2_PLACEMENT_3D('',#24831,#19983,#19984);
#17870=AXIS2_PLACEMENT_3D('',#24835,#19986,#19987);
#17871=AXIS2_PLACEMENT_3D('',#24837,#19989,#19990);
#17872=AXIS2_PLACEMENT_3D('',#24840,#19991,#19992);
#17873=AXIS2_PLACEMENT_3D('',#24844,#19994,#19995);
#17874=AXIS2_PLACEMENT_3D('',#24846,#19997,#19998);
#17875=AXIS2_PLACEMENT_3D('',#24848,#20000,#20001);
#17876=AXIS2_PLACEMENT_3D('',#24852,#20005,#20006);
#17877=AXIS2_PLACEMENT_3D('',#24853,#20007,#20008);
#17878=AXIS2_PLACEMENT_3D('',#24854,#20009,#20010);
#17879=AXIS2_PLACEMENT_3D('',#24863,#20015,#20016);
#17880=AXIS2_PLACEMENT_3D('',#24877,#20024,#20025);
#17881=AXIS2_PLACEMENT_3D('',#24883,#20029,#20030);
#17882=AXIS2_PLACEMENT_3D('',#24894,#20037,#20038);
#17883=AXIS2_PLACEMENT_3D('',#24895,#20039,#20040);
#17884=AXIS2_PLACEMENT_3D('',#24896,#20041,#20042);
#17885=AXIS2_PLACEMENT_3D('',#24897,#20043,#20044);
#17886=AXIS2_PLACEMENT_3D('',#24898,#20045,#20046);
#17887=AXIS2_PLACEMENT_3D('',#24899,#20047,#20048);
#17888=AXIS2_PLACEMENT_3D('',#24900,#20049,#20050);
#17889=AXIS2_PLACEMENT_3D('',#24901,#20051,#20052);
#17890=AXIS2_PLACEMENT_3D('',#24902,#20053,#20054);
#17891=AXIS2_PLACEMENT_3D('',#24903,#20055,#20056);
#17892=AXIS2_PLACEMENT_3D('',#24904,#20057,#20058);
#17893=AXIS2_PLACEMENT_3D('',#24908,#20060,#20061);
#17894=AXIS2_PLACEMENT_3D('',#24909,#20062,#20063);
#17895=AXIS2_PLACEMENT_3D('',#24946,#20065,#20066);
#17896=AXIS2_PLACEMENT_3D('',#24948,#20067,#20068);
#17897=AXIS2_PLACEMENT_3D('',#24951,#20070,#20071);
#17898=AXIS2_PLACEMENT_3D('',#24952,#20072,#20073);
#17899=AXIS2_PLACEMENT_3D('',#24955,#20074,#20075);
#17900=AXIS2_PLACEMENT_3D('',#24956,#20076,#20077);
#17901=AXIS2_PLACEMENT_3D('',#24959,#20079,#20080);
#17902=AXIS2_PLACEMENT_3D('',#24960,#20081,#20082);
#17903=AXIS2_PLACEMENT_3D('',#24962,#20083,#20084);
#17904=AXIS2_PLACEMENT_3D('',#24964,#20086,#20087);
#17905=AXIS2_PLACEMENT_3D('',#24966,#20088,#20089);
#17906=AXIS2_PLACEMENT_3D('',#24968,#20091,#20092);
#17907=AXIS2_PLACEMENT_3D('',#24969,#20093,#20094);
#17908=AXIS2_PLACEMENT_3D('',#24970,#20095,#20096);
#17909=AXIS2_PLACEMENT_3D('',#24971,#20097,#20098);
#17910=AXIS2_PLACEMENT_3D('',#24972,#20099,#20100);
#17911=AXIS2_PLACEMENT_3D('',#24993,#20103,#20104);
#17912=AXIS2_PLACEMENT_3D('',#25023,#20106,#20107);
#17913=AXIS2_PLACEMENT_3D('',#25053,#20109,#20110);
#17914=AXIS2_PLACEMENT_3D('',#25083,#20112,#20113);
#17915=AXIS2_PLACEMENT_3D('',#25113,#20115,#20116);
#17916=AXIS2_PLACEMENT_3D('',#25143,#20118,#20119);
#17917=AXIS2_PLACEMENT_3D('',#25173,#20121,#20122);
#17918=AXIS2_PLACEMENT_3D('',#25203,#20124,#20125);
#17919=AXIS2_PLACEMENT_3D('',#25233,#20127,#20128);
#17920=AXIS2_PLACEMENT_3D('',#25263,#20130,#20131);
#17921=AXIS2_PLACEMENT_3D('',#25293,#20133,#20134);
#17922=AXIS2_PLACEMENT_3D('',#25323,#20136,#20137);
#17923=AXIS2_PLACEMENT_3D('',#25353,#20139,#20140);
#17924=AXIS2_PLACEMENT_3D('',#25383,#20142,#20143);
#17925=AXIS2_PLACEMENT_3D('',#25413,#20145,#20146);
#17926=AXIS2_PLACEMENT_3D('',#25443,#20148,#20149);
#17927=AXIS2_PLACEMENT_3D('',#25473,#20151,#20152);
#17928=AXIS2_PLACEMENT_3D('',#25503,#20154,#20155);
#17929=AXIS2_PLACEMENT_3D('',#25533,#20157,#20158);
#17930=AXIS2_PLACEMENT_3D('',#25563,#20160,#20161);
#17931=AXIS2_PLACEMENT_3D('',#25593,#20163,#20164);
#17932=AXIS2_PLACEMENT_3D('',#25623,#20166,#20167);
#17933=AXIS2_PLACEMENT_3D('',#25653,#20169,#20170);
#17934=AXIS2_PLACEMENT_3D('',#25683,#20172,#20173);
#17935=AXIS2_PLACEMENT_3D('',#25694,#20175,#20176);
#17936=AXIS2_PLACEMENT_3D('',#25700,#20177,#20178);
#17937=AXIS2_PLACEMENT_3D('',#25705,#20180,#20181);
#17938=AXIS2_PLACEMENT_3D('',#25742,#20182,#20183);
#17939=AXIS2_PLACEMENT_3D('',#25784,#20186,#20187);
#17940=AXIS2_PLACEMENT_3D('',#25823,#20188,#20189);
#17941=AXIS2_PLACEMENT_3D('',#25899,#20191,#20192);
#17942=AXIS2_PLACEMENT_3D('',#25975,#20194,#20195);
#17943=AXIS2_PLACEMENT_3D('',#26051,#20197,#20198);
#17944=AXIS2_PLACEMENT_3D('',#26127,#20200,#20201);
#17945=AXIS2_PLACEMENT_3D('',#26205,#20203,#20204);
#17946=AXIS2_PLACEMENT_3D('',#26283,#20206,#20207);
#17947=AXIS2_PLACEMENT_3D('',#26359,#20209,#20210);
#17948=AXIS2_PLACEMENT_3D('',#26435,#20212,#20213);
#17949=AXIS2_PLACEMENT_3D('',#26511,#20215,#20216);
#17950=AXIS2_PLACEMENT_3D('',#26587,#20218,#20219);
#17951=AXIS2_PLACEMENT_3D('',#26667,#20221,#20222);
#17952=AXIS2_PLACEMENT_3D('',#26743,#20224,#20225);
#17953=AXIS2_PLACEMENT_3D('',#26819,#20227,#20228);
#17954=AXIS2_PLACEMENT_3D('',#26895,#20230,#20231);
#17955=AXIS2_PLACEMENT_3D('',#26971,#20233,#20234);
#17956=AXIS2_PLACEMENT_3D('',#27047,#20236,#20237);
#17957=AXIS2_PLACEMENT_3D('',#27127,#20239,#20240);
#17958=AXIS2_PLACEMENT_3D('',#27203,#20242,#20243);
#17959=AXIS2_PLACEMENT_3D('',#27279,#20245,#20246);
#17960=AXIS2_PLACEMENT_3D('',#27355,#20248,#20249);
#17961=AXIS2_PLACEMENT_3D('',#27431,#20251,#20252);
#17962=AXIS2_PLACEMENT_3D('',#27507,#20254,#20255);
#17963=AXIS2_PLACEMENT_3D('',#27521,#20257,#20258);
#17964=AXIS2_PLACEMENT_3D('',#27538,#20259,#20260);
#17965=AXIS2_PLACEMENT_3D('',#27541,#20262,#20263);
#17966=AXIS2_PLACEMENT_3D('',#27542,#20264,#20265);
#17967=AXIS2_PLACEMENT_3D('',#27544,#20266,#20267);
#17968=AXIS2_PLACEMENT_3D('',#27548,#20269,#20270);
#17969=AXIS2_PLACEMENT_3D('',#27585,#20271,#20272);
#17970=AXIS2_PLACEMENT_3D('',#27588,#20274,#20275);
#17971=AXIS2_PLACEMENT_3D('',#27590,#20276,#20277);
#17972=AXIS2_PLACEMENT_3D('',#27626,#20278,#20279);
#17973=AXIS2_PLACEMENT_3D('',#27627,#20280,#20281);
#17974=AXIS2_PLACEMENT_3D('',#27629,#20282,#20283);
#17975=AXIS2_PLACEMENT_3D('',#27631,#20284,#20285);
#17976=AXIS2_PLACEMENT_3D('',#27632,#20286,#20287);
#17977=AXIS2_PLACEMENT_3D('',#27633,#20288,#20289);
#17978=AXIS2_PLACEMENT_3D('',#27635,#20290,#20291);
#17979=AXIS2_PLACEMENT_3D('',#27639,#20293,#20294);
#17980=AXIS2_PLACEMENT_3D('',#27814,#20295,#20296);
#17981=AXIS2_PLACEMENT_3D('',#27817,#20298,#20299);
#17982=AXIS2_PLACEMENT_3D('',#27991,#20300,#20301);
#17983=AXIS2_PLACEMENT_3D('',#27992,#20302,#20303);
#17984=AXIS2_PLACEMENT_3D('',#27994,#20304,#20305);
#17985=AXIS2_PLACEMENT_3D('',#27996,#20306,#20307);
#17986=AXIS2_PLACEMENT_3D('',#27997,#20308,#20309);
#17987=AXIS2_PLACEMENT_3D('',#27998,#20310,#20311);
#17988=AXIS2_PLACEMENT_3D('',#28000,#20312,#20313);
#17989=AXIS2_PLACEMENT_3D('',#28002,#20315,#20316);
#17990=AXIS2_PLACEMENT_3D('',#28004,#20317,#20318);
#17991=AXIS2_PLACEMENT_3D('',#28007,#20320,#20321);
#17992=AXIS2_PLACEMENT_3D('',#28008,#20322,#20323);
#17993=AXIS2_PLACEMENT_3D('',#28085,#20324,#20325);
#17994=AXIS2_PLACEMENT_3D('',#28114,#20326,#20327);
#17995=AXIS2_PLACEMENT_3D('',#28115,#20328,#20329);
#17996=AXIS2_PLACEMENT_3D('',#28116,#20330,#20331);
#17997=AXIS2_PLACEMENT_3D('',#28117,#20332,#20333);
#17998=AXIS2_PLACEMENT_3D('',#28228,#20336,#20337);
#17999=AXIS2_PLACEMENT_3D('',#28339,#20340,#20341);
#18000=AXIS2_PLACEMENT_3D('',#28340,#20342,#20343);
#18001=AXIS2_PLACEMENT_3D('',#28343,#20346,#20347);
#18002=AXIS2_PLACEMENT_3D('',#29886,#20348,#20349);
#18003=AXIS2_PLACEMENT_3D('',#29887,#20350,#20351);
#18004=AXIS2_PLACEMENT_3D('',#29889,#20352,#20353);
#18005=AXIS2_PLACEMENT_3D('',#29892,#20355,#20356);
#18006=AXIS2_PLACEMENT_3D('',#29893,#20357,#20358);
#18007=AXIS2_PLACEMENT_3D('',#29895,#20359,#20360);
#18008=AXIS2_PLACEMENT_3D('',#29898,#20362,#20363);
#18009=AXIS2_PLACEMENT_3D('',#29899,#20364,#20365);
#18010=AXIS2_PLACEMENT_3D('',#29900,#20366,#20367);
#18011=AXIS2_PLACEMENT_3D('',#29901,#20368,#20369);
#18012=AXIS2_PLACEMENT_3D('',#29902,#20370,#20371);
#18013=AXIS2_PLACEMENT_3D('',#29903,#20372,#20373);
#18014=AXIS2_PLACEMENT_3D('',#29905,#20374,#20375);
#18015=AXIS2_PLACEMENT_3D('',#29908,#20377,#20378);
#18016=AXIS2_PLACEMENT_3D('',#29909,#20379,#20380);
#18017=AXIS2_PLACEMENT_3D('',#29911,#20381,#20382);
#18018=AXIS2_PLACEMENT_3D('',#29914,#20384,#20385);
#18019=AXIS2_PLACEMENT_3D('',#29915,#20386,#20387);
#18020=AXIS2_PLACEMENT_3D('',#29916,#20388,#20389);
#18021=AXIS2_PLACEMENT_3D('',#29917,#20390,#20391);
#18022=AXIS2_PLACEMENT_3D('',#29918,#20392,#20393);
#18023=AXIS2_PLACEMENT_3D('',#29921,#20394,#20395);
#18024=AXIS2_PLACEMENT_3D('',#29922,#20396,#20397);
#18025=AXIS2_PLACEMENT_3D('',#29924,#20398,#20399);
#18026=AXIS2_PLACEMENT_3D('',#29925,#20400,#20401);
#18027=AXIS2_PLACEMENT_3D('',#29926,#20402,#20403);
#18028=AXIS2_PLACEMENT_3D('',#29928,#20404,#20405);
#18029=AXIS2_PLACEMENT_3D('',#29930,#20406,#20407);
#18030=AXIS2_PLACEMENT_3D('',#29931,#20408,#20409);
#18031=AXIS2_PLACEMENT_3D('',#29932,#20410,#20411);
#18032=AXIS2_PLACEMENT_3D('',#29935,#20413,#20414);
#18033=AXIS2_PLACEMENT_3D('',#29936,#20415,#20416);
#18034=AXIS2_PLACEMENT_3D('',#29938,#20418,#20419);
#18035=AXIS2_PLACEMENT_3D('',#29939,#20420,#20421);
#18036=AXIS2_PLACEMENT_3D('',#29940,#20422,#20423);
#18037=AXIS2_PLACEMENT_3D('',#29941,#20424,#20425);
#18038=AXIS2_PLACEMENT_3D('',#29943,#20426,#20427);
#18039=AXIS2_PLACEMENT_3D('',#29945,#20428,#20429);
#18040=AXIS2_PLACEMENT_3D('',#29946,#20430,#20431);
#18041=AXIS2_PLACEMENT_3D('',#29947,#20432,#20433);
#18042=AXIS2_PLACEMENT_3D('',#29950,#20435,#20436);
#18043=AXIS2_PLACEMENT_3D('',#29951,#20437,#20438);
#18044=AXIS2_PLACEMENT_3D('',#29954,#20440,#20441);
#18045=AXIS2_PLACEMENT_3D('',#29955,#20442,#20443);
#18046=AXIS2_PLACEMENT_3D('',#29957,#20444,#20445);
#18047=AXIS2_PLACEMENT_3D('',#29960,#20447,#20448);
#18048=AXIS2_PLACEMENT_3D('',#29961,#20449,#20450);
#18049=AXIS2_PLACEMENT_3D('',#29964,#20452,#20453);
#18050=AXIS2_PLACEMENT_3D('',#29965,#20454,#20455);
#18051=AXIS2_PLACEMENT_3D('',#29968,#20456,#20457);
#18052=AXIS2_PLACEMENT_3D('',#29970,#20458,#20459);
#18053=AXIS2_PLACEMENT_3D('',#29971,#20460,#20461);
#18054=AXIS2_PLACEMENT_3D('',#29974,#20463,#20464);
#18055=AXIS2_PLACEMENT_3D('',#29975,#20465,#20466);
#18056=AXIS2_PLACEMENT_3D('',#29976,#20467,#20468);
#18057=AXIS2_PLACEMENT_3D('',#29977,#20469,#20470);
#18058=AXIS2_PLACEMENT_3D('',#29978,#20471,#20472);
#18059=AXIS2_PLACEMENT_3D('',#29979,#20473,#20474);
#18060=AXIS2_PLACEMENT_3D('',#29981,#20475,#20476);
#18061=AXIS2_PLACEMENT_3D('',#29984,#20478,#20479);
#18062=AXIS2_PLACEMENT_3D('',#29985,#20480,#20481);
#18063=AXIS2_PLACEMENT_3D('',#29988,#20482,#20483);
#18064=AXIS2_PLACEMENT_3D('',#29990,#20484,#20485);
#18065=AXIS2_PLACEMENT_3D('',#29991,#20486,#20487);
#18066=AXIS2_PLACEMENT_3D('',#29992,#20488,#20489);
#18067=AXIS2_PLACEMENT_3D('',#29994,#20490,#20491);
#18068=AXIS2_PLACEMENT_3D('',#29996,#20492,#20493);
#18069=AXIS2_PLACEMENT_3D('',#29997,#20494,#20495);
#18070=AXIS2_PLACEMENT_3D('',#29998,#20496,#20497);
#18071=AXIS2_PLACEMENT_3D('',#30013,#20499,#20500);
#18072=AXIS2_PLACEMENT_3D('',#30026,#20502,#20503);
#18073=AXIS2_PLACEMENT_3D('',#30029,#20504,#20505);
#18074=AXIS2_PLACEMENT_3D('',#30158,#20506,#20507);
#18075=AXIS2_PLACEMENT_3D('',#30296,#20508,#20509);
#18076=AXIS2_PLACEMENT_3D('',#30303,#20510,#20511);
#18077=AXIS2_PLACEMENT_3D('',#30305,#20512,#20513);
#18078=AXIS2_PLACEMENT_3D('',#30306,#20514,#20515);
#18079=AXIS2_PLACEMENT_3D('',#30307,#20516,#20517);
#18080=AXIS2_PLACEMENT_3D('',#30445,#20518,#20519);
#18081=AXIS2_PLACEMENT_3D('',#30448,#20521,#20522);
#18082=AXIS2_PLACEMENT_3D('',#30450,#20523,#20524);
#18083=AXIS2_PLACEMENT_3D('',#30593,#20525,#20526);
#18084=AXIS2_PLACEMENT_3D('',#30595,#20527,#20528);
#18085=AXIS2_PLACEMENT_3D('',#30625,#20529,#20530);
#18086=AXIS2_PLACEMENT_3D('',#30626,#20531,#20532);
#18087=AXIS2_PLACEMENT_3D('',#30642,#20535,#20536);
#18088=AXIS2_PLACEMENT_3D('',#30655,#20538,#20539);
#18089=AXIS2_PLACEMENT_3D('',#30656,#20540,#20541);
#18090=AXIS2_PLACEMENT_3D('',#30657,#20542,#20543);
#18091=AXIS2_PLACEMENT_3D('',#30658,#20544,#20545);
#18092=AXIS2_PLACEMENT_3D('',#30659,#20546,#20547);
#18093=AXIS2_PLACEMENT_3D('',#30660,#20548,#20549);
#18094=AXIS2_PLACEMENT_3D('',#31236,#20552,#20553);
#18095=AXIS2_PLACEMENT_3D('',#31238,#20554,#20555);
#18096=AXIS2_PLACEMENT_3D('',#31241,#20557,#20558);
#18097=AXIS2_PLACEMENT_3D('',#31242,#20559,#20560);
#18098=AXIS2_PLACEMENT_3D('',#31244,#20561,#20562);
#18099=AXIS2_PLACEMENT_3D('',#31247,#20564,#20565);
#18100=AXIS2_PLACEMENT_3D('',#31248,#20566,#20567);
#18101=AXIS2_PLACEMENT_3D('',#31250,#20568,#20569);
#18102=AXIS2_PLACEMENT_3D('',#31252,#20571,#20572);
#18103=AXIS2_PLACEMENT_3D('',#31254,#20574,#20575);
#18104=AXIS2_PLACEMENT_3D('',#31327,#20576,#20577);
#18105=AXIS2_PLACEMENT_3D('',#31376,#20578,#20579);
#18106=AXIS2_PLACEMENT_3D('',#31389,#20580,#20581);
#18107=AXIS2_PLACEMENT_3D('',#31390,#20582,#20583);
#18108=AXIS2_PLACEMENT_3D('',#31391,#20584,#20585);
#18109=AXIS2_PLACEMENT_3D('',#31392,#20586,#20587);
#18110=AXIS2_PLACEMENT_3D('',#31393,#20588,#20589);
#18111=AXIS2_PLACEMENT_3D('',#31394,#20590,#20591);
#18112=AXIS2_PLACEMENT_3D('',#31395,#20592,#20593);
#18113=AXIS2_PLACEMENT_3D('',#31396,#20594,#20595);
#18114=AXIS2_PLACEMENT_3D('',#31397,#20596,#20597);
#18115=AXIS2_PLACEMENT_3D('',#31398,#20598,#20599);
#18116=AXIS2_PLACEMENT_3D('',#31399,#20600,#20601);
#18117=AXIS2_PLACEMENT_3D('',#31864,#20602,#20603);
#18118=AXIS2_PLACEMENT_3D('',#31865,#20604,#20605);
#18119=AXIS2_PLACEMENT_3D('',#31866,#20606,#20607);
#18120=AXIS2_PLACEMENT_3D('',#31867,#20608,#20609);
#18121=AXIS2_PLACEMENT_3D('',#31868,#20610,#20611);
#18122=AXIS2_PLACEMENT_3D('',#31869,#20612,#20613);
#18123=AXIS2_PLACEMENT_3D('',#31870,#20614,#20615);
#18124=AXIS2_PLACEMENT_3D('',#31871,#20616,#20617);
#18125=AXIS2_PLACEMENT_3D('',#31884,#20618,#20619);
#18126=AXIS2_PLACEMENT_3D('',#31927,#20620,#20621);
#18127=AXIS2_PLACEMENT_3D('',#32000,#20622,#20623);
#18128=AXIS2_PLACEMENT_3D('',#32001,#20624,#20625);
#18129=AXIS2_PLACEMENT_3D('',#32004,#20626,#20627);
#18130=AXIS2_PLACEMENT_3D('',#32006,#20628,#20629);
#18131=AXIS2_PLACEMENT_3D('',#32008,#20630,#20631);
#18132=AXIS2_PLACEMENT_3D('',#32009,#20632,#20633);
#18133=AXIS2_PLACEMENT_3D('',#32010,#20634,#20635);
#18134=AXIS2_PLACEMENT_3D('',#32012,#20636,#20637);
#18135=AXIS2_PLACEMENT_3D('',#32015,#20639,#20640);
#18136=AXIS2_PLACEMENT_3D('',#32016,#20641,#20642);
#18137=AXIS2_PLACEMENT_3D('',#32017,#20643,#20644);
#18138=AXIS2_PLACEMENT_3D('',#32018,#20645,#20646);
#18139=AXIS2_PLACEMENT_3D('',#32019,#20647,#20648);
#18140=AXIS2_PLACEMENT_3D('',#32020,#20649,#20650);
#18141=AXIS2_PLACEMENT_3D('',#32023,#20652,#20653);
#18142=AXIS2_PLACEMENT_3D('',#32024,#20654,#20655);
#18143=AXIS2_PLACEMENT_3D('',#32027,#20657,#20658);
#18144=AXIS2_PLACEMENT_3D('',#32028,#20659,#20660);
#18145=AXIS2_PLACEMENT_3D('',#32031,#20662,#20663);
#18146=AXIS2_PLACEMENT_3D('',#32032,#20664,#20665);
#18147=AXIS2_PLACEMENT_3D('',#32033,#20666,#20667);
#18148=AXIS2_PLACEMENT_3D('',#32034,#20668,#20669);
#18149=AXIS2_PLACEMENT_3D('',#32035,#20670,#20671);
#18150=AXIS2_PLACEMENT_3D('',#32036,#20672,#20673);
#18151=AXIS2_PLACEMENT_3D('',#32039,#20674,#20675);
#18152=AXIS2_PLACEMENT_3D('',#32067,#20676,#20677);
#18153=AXIS2_PLACEMENT_3D('',#32069,#20678,#20679);
#18154=AXIS2_PLACEMENT_3D('',#32131,#20680,#20681);
#18155=AXIS2_PLACEMENT_3D('',#32134,#20682,#20683);
#18156=AXIS2_PLACEMENT_3D('',#32138,#20685,#20686);
#18157=AXIS2_PLACEMENT_3D('',#32159,#20687,#20688);
#18158=AXIS2_PLACEMENT_3D('',#32273,#20690,#20691);
#18159=AXIS2_PLACEMENT_3D('',#32275,#20692,#20693);
#18160=AXIS2_PLACEMENT_3D('',#32278,#20695,#20696);
#18161=AXIS2_PLACEMENT_3D('',#32279,#20697,#20698);
#18162=AXIS2_PLACEMENT_3D('',#32282,#20699,#20700);
#18163=AXIS2_PLACEMENT_3D('',#32382,#20701,#20702);
#18164=AXIS2_PLACEMENT_3D('',#32482,#20703,#20704);
#18165=AXIS2_PLACEMENT_3D('',#32483,#20705,#20706);
#18166=AXIS2_PLACEMENT_3D('',#32484,#20707,#20708);
#18167=AXIS2_PLACEMENT_3D('',#32485,#20709,#20710);
#18168=AXIS2_PLACEMENT_3D('',#32486,#20711,#20712);
#18169=AXIS2_PLACEMENT_3D('',#32487,#20713,#20714);
#18170=AXIS2_PLACEMENT_3D('',#32488,#20715,#20716);
#18171=AXIS2_PLACEMENT_3D('',#32491,#20718,#20719);
#18172=AXIS2_PLACEMENT_3D('',#32492,#20720,#20721);
#18173=AXIS2_PLACEMENT_3D('',#32494,#20722,#20723);
#18174=AXIS2_PLACEMENT_3D('',#32497,#20725,#20726);
#18175=AXIS2_PLACEMENT_3D('',#32533,#20727,#20728);
#18176=AXIS2_PLACEMENT_3D('',#32535,#20729,#20730);
#18177=AXIS2_PLACEMENT_3D('',#32537,#20731,#20732);
#18178=AXIS2_PLACEMENT_3D('',#32539,#20733,#20734);
#18179=AXIS2_PLACEMENT_3D('',#32540,#20735,#20736);
#18180=AXIS2_PLACEMENT_3D('',#32542,#20737,#20738);
#18181=AXIS2_PLACEMENT_3D('',#32543,#20739,#20740);
#18182=AXIS2_PLACEMENT_3D('',#32544,#20741,#20742);
#18183=AXIS2_PLACEMENT_3D('',#32545,#20743,#20744);
#18184=AXIS2_PLACEMENT_3D('',#32607,#20746,#20747);
#18185=AXIS2_PLACEMENT_3D('',#32608,#20748,#20749);
#18186=AXIS2_PLACEMENT_3D('',#32615,#20750,#20751);
#18187=AXIS2_PLACEMENT_3D('',#32679,#20753,#20754);
#18188=AXIS2_PLACEMENT_3D('',#32680,#20755,#20756);
#18189=AXIS2_PLACEMENT_3D('',#32681,#20757,#20758);
#18190=AXIS2_PLACEMENT_3D('',#32682,#20759,#20760);
#18191=AXIS2_PLACEMENT_3D('',#32749,#20761,#20762);
#18192=AXIS2_PLACEMENT_3D('',#32750,#20763,#20764);
#18193=AXIS2_PLACEMENT_3D('',#32769,#20765,#20766);
#18194=AXIS2_PLACEMENT_3D('',#32906,#20767,#20768);
#18195=AXIS2_PLACEMENT_3D('',#32907,#20769,#20770);
#18196=AXIS2_PLACEMENT_3D('',#32974,#20771,#20772);
#18197=AXIS2_PLACEMENT_3D('',#32975,#20773,#20774);
#18198=AXIS2_PLACEMENT_3D('',#32978,#20775,#20776);
#18199=AXIS2_PLACEMENT_3D('',#32980,#20777,#20778);
#18200=AXIS2_PLACEMENT_3D('',#32982,#20779,#20780);
#18201=AXIS2_PLACEMENT_3D('',#32983,#20781,#20782);
#18202=AXIS2_PLACEMENT_3D('',#32984,#20783,#20784);
#18203=AXIS2_PLACEMENT_3D('',#32986,#20785,#20786);
#18204=AXIS2_PLACEMENT_3D('',#32989,#20788,#20789);
#18205=AXIS2_PLACEMENT_3D('',#32990,#20790,#20791);
#18206=AXIS2_PLACEMENT_3D('',#32991,#20792,#20793);
#18207=AXIS2_PLACEMENT_3D('',#32992,#20794,#20795);
#18208=AXIS2_PLACEMENT_3D('',#32993,#20796,#20797);
#18209=AXIS2_PLACEMENT_3D('',#32994,#20798,#20799);
#18210=AXIS2_PLACEMENT_3D('',#32997,#20801,#20802);
#18211=AXIS2_PLACEMENT_3D('',#32998,#20803,#20804);
#18212=AXIS2_PLACEMENT_3D('',#33001,#20806,#20807);
#18213=AXIS2_PLACEMENT_3D('',#33002,#20808,#20809);
#18214=AXIS2_PLACEMENT_3D('',#33005,#20811,#20812);
#18215=AXIS2_PLACEMENT_3D('',#33006,#20813,#20814);
#18216=AXIS2_PLACEMENT_3D('',#33007,#20815,#20816);
#18217=AXIS2_PLACEMENT_3D('',#33008,#20817,#20818);
#18218=AXIS2_PLACEMENT_3D('',#33009,#20819,#20820);
#18219=AXIS2_PLACEMENT_3D('',#33010,#20821,#20822);
#18220=AXIS2_PLACEMENT_3D('',#33013,#20823,#20824);
#18221=AXIS2_PLACEMENT_3D('',#33014,#20825,#20826);
#18222=AXIS2_PLACEMENT_3D('',#33016,#20827,#20828);
#18223=AXIS2_PLACEMENT_3D('',#33017,#20829,#20830);
#18224=AXIS2_PLACEMENT_3D('',#33018,#20831,#20832);
#18225=AXIS2_PLACEMENT_3D('',#33020,#20833,#20834);
#18226=AXIS2_PLACEMENT_3D('',#33023,#20836,#20837);
#18227=AXIS2_PLACEMENT_3D('',#33024,#20838,#20839);
#18228=AXIS2_PLACEMENT_3D('',#33027,#20840,#20841);
#18229=AXIS2_PLACEMENT_3D('',#33028,#20842,#20843);
#18230=AXIS2_PLACEMENT_3D('',#33030,#20845,#20846);
#18231=AXIS2_PLACEMENT_3D('',#33034,#20848,#20849);
#18232=AXIS2_PLACEMENT_3D('',#33035,#20850,#20851);
#18233=AXIS2_PLACEMENT_3D('',#33036,#20852,#20853);
#18234=AXIS2_PLACEMENT_3D('',#33038,#20854,#20855);
#18235=AXIS2_PLACEMENT_3D('',#33040,#20857,#20858);
#18236=AXIS2_PLACEMENT_3D('',#33042,#20859,#20860);
#18237=AXIS2_PLACEMENT_3D('',#33045,#20862,#20863);
#18238=AXIS2_PLACEMENT_3D('',#33046,#20864,#20865);
#18239=AXIS2_PLACEMENT_3D('',#33049,#20867,#20868);
#18240=AXIS2_PLACEMENT_3D('',#33050,#20869,#20870);
#18241=AXIS2_PLACEMENT_3D('',#33051,#20871,#20872);
#18242=AXIS2_PLACEMENT_3D('',#33052,#20873,#20874);
#18243=AXIS2_PLACEMENT_3D('',#33053,#20875,#20876);
#18244=AXIS2_PLACEMENT_3D('',#33054,#20877,#20878);
#18245=AXIS2_PLACEMENT_3D('',#33055,#20879,#20880);
#18246=AXIS2_PLACEMENT_3D('',#33058,#20881,#20882);
#18247=AXIS2_PLACEMENT_3D('',#33060,#20883,#20884);
#18248=AXIS2_PLACEMENT_3D('',#33062,#20885,#20886);
#18249=AXIS2_PLACEMENT_3D('',#33063,#20887,#20888);
#18250=AXIS2_PLACEMENT_3D('',#33064,#20889,#20890);
#18251=AXIS2_PLACEMENT_3D('',#33067,#20891,#20892);
#18252=AXIS2_PLACEMENT_3D('',#33071,#20894,#20895);
#18253=AXIS2_PLACEMENT_3D('',#33073,#20897,#20898);
#18254=AXIS2_PLACEMENT_3D('',#33075,#20899,#20900);
#18255=AXIS2_PLACEMENT_3D('',#33077,#20901,#20902);
#18256=AXIS2_PLACEMENT_3D('',#33079,#20903,#20904);
#18257=AXIS2_PLACEMENT_3D('',#33080,#20905,#20906);
#18258=AXIS2_PLACEMENT_3D('',#33081,#20907,#20908);
#18259=AXIS2_PLACEMENT_3D('',#33084,#20909,#20910);
#18260=AXIS2_PLACEMENT_3D('',#33086,#20911,#20912);
#18261=AXIS2_PLACEMENT_3D('',#33088,#20913,#20914);
#18262=AXIS2_PLACEMENT_3D('',#33089,#20915,#20916);
#18263=AXIS2_PLACEMENT_3D('',#33090,#20917,#20918);
#18264=AXIS2_PLACEMENT_3D('',#33093,#20919,#20920);
#18265=AXIS2_PLACEMENT_3D('',#33097,#20922,#20923);
#18266=AXIS2_PLACEMENT_3D('',#33099,#20925,#20926);
#18267=AXIS2_PLACEMENT_3D('',#33101,#20927,#20928);
#18268=AXIS2_PLACEMENT_3D('',#33103,#20929,#20930);
#18269=AXIS2_PLACEMENT_3D('',#33105,#20931,#20932);
#18270=AXIS2_PLACEMENT_3D('',#33106,#20933,#20934);
#18271=AXIS2_PLACEMENT_3D('',#33107,#20935,#20936);
#18272=AXIS2_PLACEMENT_3D('',#33110,#20937,#20938);
#18273=AXIS2_PLACEMENT_3D('',#33114,#20940,#20941);
#18274=AXIS2_PLACEMENT_3D('',#33116,#20943,#20944);
#18275=AXIS2_PLACEMENT_3D('',#33118,#20945,#20946);
#18276=AXIS2_PLACEMENT_3D('',#33120,#20947,#20948);
#18277=AXIS2_PLACEMENT_3D('',#33122,#20949,#20950);
#18278=AXIS2_PLACEMENT_3D('',#33123,#20951,#20952);
#18279=AXIS2_PLACEMENT_3D('',#33124,#20953,#20954);
#18280=AXIS2_PLACEMENT_3D('',#33127,#20955,#20956);
#18281=AXIS2_PLACEMENT_3D('',#33129,#20957,#20958);
#18282=AXIS2_PLACEMENT_3D('',#33131,#20959,#20960);
#18283=AXIS2_PLACEMENT_3D('',#33132,#20961,#20962);
#18284=AXIS2_PLACEMENT_3D('',#33133,#20963,#20964);
#18285=AXIS2_PLACEMENT_3D('',#33136,#20965,#20966);
#18286=AXIS2_PLACEMENT_3D('',#33139,#20968,#20969);
#18287=AXIS2_PLACEMENT_3D('',#33141,#20971,#20972);
#18288=AXIS2_PLACEMENT_3D('',#33144,#20974,#20975);
#18289=AXIS2_PLACEMENT_3D('',#33145,#20976,#20977);
#18290=AXIS2_PLACEMENT_3D('',#33148,#20979,#20980);
#18291=AXIS2_PLACEMENT_3D('',#33149,#20981,#20982);
#18292=AXIS2_PLACEMENT_3D('',#33153,#20984,#20985);
#18293=AXIS2_PLACEMENT_3D('',#33155,#20987,#20988);
#18294=AXIS2_PLACEMENT_3D('',#33157,#20989,#20990);
#18295=AXIS2_PLACEMENT_3D('',#33160,#20992,#20993);
#18296=AXIS2_PLACEMENT_3D('',#33161,#20994,#20995);
#18297=AXIS2_PLACEMENT_3D('',#33163,#20996,#20997);
#18298=AXIS2_PLACEMENT_3D('',#33166,#20999,#21000);
#18299=AXIS2_PLACEMENT_3D('',#33167,#21001,#21002);
#18300=AXIS2_PLACEMENT_3D('',#33170,#21003,#21004);
#18301=AXIS2_PLACEMENT_3D('',#33174,#21006,#21007);
#18302=AXIS2_PLACEMENT_3D('',#33176,#21009,#21010);
#18303=AXIS2_PLACEMENT_3D('',#33178,#21011,#21012);
#18304=AXIS2_PLACEMENT_3D('',#33181,#21014,#21015);
#18305=AXIS2_PLACEMENT_3D('',#33182,#21016,#21017);
#18306=AXIS2_PLACEMENT_3D('',#33183,#21018,#21019);
#18307=AXIS2_PLACEMENT_3D('',#33184,#21020,#21021);
#18308=AXIS2_PLACEMENT_3D('',#33185,#21022,#21023);
#18309=AXIS2_PLACEMENT_3D('',#33187,#21024,#21025);
#18310=AXIS2_PLACEMENT_3D('',#33190,#21027,#21028);
#18311=AXIS2_PLACEMENT_3D('',#33191,#21029,#21030);
#18312=AXIS2_PLACEMENT_3D('',#33194,#21031,#21032);
#18313=AXIS2_PLACEMENT_3D('',#33198,#21034,#21035);
#18314=AXIS2_PLACEMENT_3D('',#33200,#21037,#21038);
#18315=AXIS2_PLACEMENT_3D('',#33203,#21039,#21040);
#18316=AXIS2_PLACEMENT_3D('',#33204,#21041,#21042);
#18317=AXIS2_PLACEMENT_3D('',#33205,#21043,#21044);
#18318=AXIS2_PLACEMENT_3D('',#33206,#21045,#21046);
#18319=AXIS2_PLACEMENT_3D('',#33209,#21047,#21048);
#18320=AXIS2_PLACEMENT_3D('',#33210,#21049,#21050);
#18321=AXIS2_PLACEMENT_3D('',#33211,#21051,#21052);
#18322=AXIS2_PLACEMENT_3D('',#33212,#21053,#21054);
#18323=AXIS2_PLACEMENT_3D('',#33214,#21055,#21056);
#18324=AXIS2_PLACEMENT_3D('',#33215,#21057,#21058);
#18325=AXIS2_PLACEMENT_3D('',#33216,#21059,#21060);
#18326=AXIS2_PLACEMENT_3D('',#33217,#21061,#21062);
#18327=AXIS2_PLACEMENT_3D('',#33218,#21063,#21064);
#18328=AXIS2_PLACEMENT_3D('',#33219,#21065,#21066);
#18329=AXIS2_PLACEMENT_3D('',#33220,#21067,#21068);
#18330=AXIS2_PLACEMENT_3D('',#33221,#21069,#21070);
#18331=AXIS2_PLACEMENT_3D('',#33224,#21071,#21072);
#18332=AXIS2_PLACEMENT_3D('',#33225,#21073,#21074);
#18333=AXIS2_PLACEMENT_3D('',#33227,#21075,#21076);
#18334=AXIS2_PLACEMENT_3D('',#33228,#21077,#21078);
#18335=AXIS2_PLACEMENT_3D('',#33229,#21079,#21080);
#18336=AXIS2_PLACEMENT_3D('',#33230,#21081,#21082);
#18337=AXIS2_PLACEMENT_3D('',#33231,#21083,#21084);
#18338=AXIS2_PLACEMENT_3D('',#33232,#21085,#21086);
#18339=AXIS2_PLACEMENT_3D('',#33233,#21087,#21088);
#18340=AXIS2_PLACEMENT_3D('',#33234,#21089,#21090);
#18341=AXIS2_PLACEMENT_3D('',#33235,#21091,#21092);
#18342=AXIS2_PLACEMENT_3D('',#33236,#21093,#21094);
#18343=AXIS2_PLACEMENT_3D('',#33237,#21095,#21096);
#18344=AXIS2_PLACEMENT_3D('',#33239,#21097,#21098);
#18345=AXIS2_PLACEMENT_3D('',#33240,#21099,#21100);
#18346=AXIS2_PLACEMENT_3D('',#33241,#21101,#21102);
#18347=AXIS2_PLACEMENT_3D('',#33242,#21103,#21104);
#18348=AXIS2_PLACEMENT_3D('',#33245,#21105,#21106);
#18349=AXIS2_PLACEMENT_3D('',#33246,#21107,#21108);
#18350=AXIS2_PLACEMENT_3D('',#33247,#21109,#21110);
#18351=AXIS2_PLACEMENT_3D('',#33248,#21111,#21112);
#18352=AXIS2_PLACEMENT_3D('',#33250,#21113,#21114);
#18353=AXIS2_PLACEMENT_3D('',#33252,#21115,#21116);
#18354=AXIS2_PLACEMENT_3D('',#33254,#21117,#21118);
#18355=AXIS2_PLACEMENT_3D('',#33255,#21119,#21120);
#18356=AXIS2_PLACEMENT_3D('',#33256,#21121,#21122);
#18357=AXIS2_PLACEMENT_3D('',#33257,#21123,#21124);
#18358=AXIS2_PLACEMENT_3D('',#33258,#21125,#21126);
#18359=AXIS2_PLACEMENT_3D('',#33259,#21127,#21128);
#18360=AXIS2_PLACEMENT_3D('',#33260,#21129,#21130);
#18361=AXIS2_PLACEMENT_3D('',#33261,#21131,#21132);
#18362=AXIS2_PLACEMENT_3D('',#33264,#21135,#21136);
#18363=AXIS2_PLACEMENT_3D('',#33265,#21137,#21138);
#18364=AXIS2_PLACEMENT_3D('',#33267,#21139,#21140);
#18365=AXIS2_PLACEMENT_3D('',#33269,#21141,#21142);
#18366=AXIS2_PLACEMENT_3D('',#33270,#21143,#21144);
#18367=AXIS2_PLACEMENT_3D('',#33271,#21145,#21146);
#18368=AXIS2_PLACEMENT_3D('',#33272,#21147,#21148);
#18369=AXIS2_PLACEMENT_3D('',#33273,#21149,#21150);
#18370=AXIS2_PLACEMENT_3D('',#33274,#21151,#21152);
#18371=AXIS2_PLACEMENT_3D('',#33275,#21153,#21154);
#18372=AXIS2_PLACEMENT_3D('',#33276,#21155,#21156);
#18373=AXIS2_PLACEMENT_3D('',#33277,#21157,#21158);
#18374=AXIS2_PLACEMENT_3D('',#33278,#21159,#21160);
#18375=AXIS2_PLACEMENT_3D('',#33279,#21161,#21162);
#18376=AXIS2_PLACEMENT_3D('',#33283,#21164,#21165);
#18377=AXIS2_PLACEMENT_3D('',#33285,#21167,#21168);
#18378=AXIS2_PLACEMENT_3D('',#33288,#21170,#21171);
#18379=AXIS2_PLACEMENT_3D('',#33289,#21172,#21173);
#18380=AXIS2_PLACEMENT_3D('',#33292,#21175,#21176);
#18381=AXIS2_PLACEMENT_3D('',#33293,#21177,#21178);
#18382=AXIS2_PLACEMENT_3D('',#33294,#21179,#21180);
#18383=AXIS2_PLACEMENT_3D('',#33295,#21181,#21182);
#18384=AXIS2_PLACEMENT_3D('',#33296,#21183,#21184);
#18385=AXIS2_PLACEMENT_3D('',#33297,#21185,#21186);
#18386=AXIS2_PLACEMENT_3D('',#33298,#21187,#21188);
#18387=AXIS2_PLACEMENT_3D('',#33299,#21189,#21190);
#18388=AXIS2_PLACEMENT_3D('',#33300,#21191,#21192);
#18389=AXIS2_PLACEMENT_3D('',#33301,#21193,#21194);
#18390=AXIS2_PLACEMENT_3D('',#33302,#21195,#21196);
#18391=AXIS2_PLACEMENT_3D('',#33303,#21197,#21198);
#18392=AXIS2_PLACEMENT_3D('',#33304,#21199,#21200);
#18393=AXIS2_PLACEMENT_3D('',#33305,#21201,#21202);
#18394=AXIS2_PLACEMENT_3D('',#33306,#21203,#21204);
#18395=AXIS2_PLACEMENT_3D('',#33307,#21205,#21206);
#18396=AXIS2_PLACEMENT_3D('',#33308,#21207,#21208);
#18397=AXIS2_PLACEMENT_3D('',#33309,#21209,#21210);
#18398=AXIS2_PLACEMENT_3D('',#33310,#21211,#21212);
#18399=AXIS2_PLACEMENT_3D('',#33311,#21213,#21214);
#18400=AXIS2_PLACEMENT_3D('',#33312,#21215,#21216);
#18401=AXIS2_PLACEMENT_3D('',#33313,#21217,#21218);
#18402=AXIS2_PLACEMENT_3D('',#33314,#21219,#21220);
#18403=AXIS2_PLACEMENT_3D('',#33315,#21221,#21222);
#18404=AXIS2_PLACEMENT_3D('',#33316,#21223,#21224);
#18405=AXIS2_PLACEMENT_3D('',#33317,#21225,#21226);
#18406=AXIS2_PLACEMENT_3D('',#33318,#21227,#21228);
#18407=AXIS2_PLACEMENT_3D('',#33319,#21229,#21230);
#18408=AXIS2_PLACEMENT_3D('',#33320,#21231,#21232);
#18409=AXIS2_PLACEMENT_3D('',#33321,#21233,#21234);
#18410=AXIS2_PLACEMENT_3D('',#33322,#21235,#21236);
#18411=AXIS2_PLACEMENT_3D('',#33323,#21237,#21238);
#18412=AXIS2_PLACEMENT_3D('',#33324,#21239,#21240);
#18413=AXIS2_PLACEMENT_3D('',#33325,#21241,#21242);
#18414=AXIS2_PLACEMENT_3D('',#33326,#21243,#21244);
#18415=AXIS2_PLACEMENT_3D('',#33327,#21245,#21246);
#18416=AXIS2_PLACEMENT_3D('',#33328,#21247,#21248);
#18417=AXIS2_PLACEMENT_3D('',#33329,#21249,#21250);
#18418=AXIS2_PLACEMENT_3D('',#33330,#21251,#21252);
#18419=AXIS2_PLACEMENT_3D('',#33331,#21253,#21254);
#18420=AXIS2_PLACEMENT_3D('',#33332,#21255,#21256);
#18421=AXIS2_PLACEMENT_3D('',#33333,#21257,#21258);
#18422=AXIS2_PLACEMENT_3D('',#33334,#21259,#21260);
#18423=AXIS2_PLACEMENT_3D('',#33335,#21261,#21262);
#18424=AXIS2_PLACEMENT_3D('',#33336,#21263,#21264);
#18425=AXIS2_PLACEMENT_3D('',#33337,#21265,#21266);
#18426=AXIS2_PLACEMENT_3D('',#33338,#21267,#21268);
#18427=AXIS2_PLACEMENT_3D('',#33339,#21269,#21270);
#18428=AXIS2_PLACEMENT_3D('',#33340,#21271,#21272);
#18429=AXIS2_PLACEMENT_3D('',#33341,#21273,#21274);
#18430=AXIS2_PLACEMENT_3D('',#33342,#21275,#21276);
#18431=AXIS2_PLACEMENT_3D('',#33343,#21277,#21278);
#18432=AXIS2_PLACEMENT_3D('',#33344,#21279,#21280);
#18433=AXIS2_PLACEMENT_3D('',#33345,#21281,#21282);
#18434=AXIS2_PLACEMENT_3D('',#33346,#21283,#21284);
#18435=AXIS2_PLACEMENT_3D('',#33347,#21285,#21286);
#18436=AXIS2_PLACEMENT_3D('',#33348,#21287,#21288);
#18437=AXIS2_PLACEMENT_3D('',#33349,#21289,#21290);
#18438=AXIS2_PLACEMENT_3D('',#33350,#21291,#21292);
#18439=AXIS2_PLACEMENT_3D('',#33351,#21293,#21294);
#18440=AXIS2_PLACEMENT_3D('',#33352,#21295,#21296);
#18441=AXIS2_PLACEMENT_3D('',#33353,#21297,#21298);
#18442=AXIS2_PLACEMENT_3D('',#33354,#21299,#21300);
#18443=AXIS2_PLACEMENT_3D('',#33355,#21301,#21302);
#18444=AXIS2_PLACEMENT_3D('',#33356,#21303,#21304);
#18445=AXIS2_PLACEMENT_3D('',#33357,#21305,#21306);
#18446=AXIS2_PLACEMENT_3D('',#33358,#21307,#21308);
#18447=AXIS2_PLACEMENT_3D('',#33359,#21309,#21310);
#18448=AXIS2_PLACEMENT_3D('',#33360,#21311,#21312);
#18449=AXIS2_PLACEMENT_3D('',#33362,#21313,#21314);
#18450=AXIS2_PLACEMENT_3D('',#33365,#21316,#21317);
#18451=AXIS2_PLACEMENT_3D('',#33366,#21318,#21319);
#18452=AXIS2_PLACEMENT_3D('',#33369,#21320,#21321);
#18453=AXIS2_PLACEMENT_3D('',#33370,#21322,#21323);
#18454=AXIS2_PLACEMENT_3D('',#33373,#21325,#21326);
#18455=AXIS2_PLACEMENT_3D('',#33374,#21327,#21328);
#18456=AXIS2_PLACEMENT_3D('',#33377,#21329,#21330);
#18457=AXIS2_PLACEMENT_3D('',#33378,#21331,#21332);
#18458=AXIS2_PLACEMENT_3D('',#33381,#21334,#21335);
#18459=AXIS2_PLACEMENT_3D('',#33382,#21336,#21337);
#18460=AXIS2_PLACEMENT_3D('',#33384,#21338,#21339);
#18461=AXIS2_PLACEMENT_3D('',#33387,#21341,#21342);
#18462=AXIS2_PLACEMENT_3D('',#33388,#21343,#21344);
#18463=AXIS2_PLACEMENT_3D('',#33391,#21345,#21346);
#18464=AXIS2_PLACEMENT_3D('',#33397,#21347,#21348);
#18465=AXIS2_PLACEMENT_3D('',#33401,#21349,#21350);
#18466=AXIS2_PLACEMENT_3D('',#33404,#21351,#21352);
#18467=AXIS2_PLACEMENT_3D('',#33405,#21353,#21354);
#18468=AXIS2_PLACEMENT_3D('',#33408,#21356,#21357);
#18469=AXIS2_PLACEMENT_3D('',#33409,#21358,#21359);
#18470=AXIS2_PLACEMENT_3D('',#33412,#21360,#21361);
#18471=AXIS2_PLACEMENT_3D('',#33413,#21362,#21363);
#18472=AXIS2_PLACEMENT_3D('',#33416,#21365,#21366);
#18473=AXIS2_PLACEMENT_3D('',#33417,#21367,#21368);
#18474=AXIS2_PLACEMENT_3D('',#33419,#21369,#21370);
#18475=AXIS2_PLACEMENT_3D('',#33422,#21372,#21373);
#18476=AXIS2_PLACEMENT_3D('',#33423,#21374,#21375);
#18477=AXIS2_PLACEMENT_3D('',#33425,#21376,#21377);
#18478=AXIS2_PLACEMENT_3D('',#33428,#21379,#21380);
#18479=AXIS2_PLACEMENT_3D('',#33429,#21381,#21382);
#18480=AXIS2_PLACEMENT_3D('',#33432,#21383,#21384);
#18481=AXIS2_PLACEMENT_3D('',#33438,#21385,#21386);
#18482=AXIS2_PLACEMENT_3D('',#33442,#21387,#21388);
#18483=AXIS2_PLACEMENT_3D('',#33446,#21390,#21391);
#18484=AXIS2_PLACEMENT_3D('',#33475,#21392,#21393);
#18485=AXIS2_PLACEMENT_3D('',#33476,#21394,#21395);
#18486=AXIS2_PLACEMENT_3D('',#33478,#21396,#21397);
#18487=AXIS2_PLACEMENT_3D('',#33480,#21399,#21400);
#18488=AXIS2_PLACEMENT_3D('',#33482,#21402,#21403);
#18489=AXIS2_PLACEMENT_3D('',#33486,#21407,#21408);
#18490=AXIS2_PLACEMENT_3D('',#33488,#21410,#21411);
#18491=AXIS2_PLACEMENT_3D('',#33490,#21413,#21414);
#18492=AXIS2_PLACEMENT_3D('',#33499,#21419,#21420);
#18493=AXIS2_PLACEMENT_3D('',#33508,#21425,#21426);
#18494=AXIS2_PLACEMENT_3D('',#33512,#21428,#21429);
#18495=AXIS2_PLACEMENT_3D('',#33533,#21440,#21441);
#18496=AXIS2_PLACEMENT_3D('',#33535,#21443,#21444);
#18497=AXIS2_PLACEMENT_3D('',#33541,#21448,#21449);
#18498=AXIS2_PLACEMENT_3D('',#33547,#21452,#21453);
#18499=AXIS2_PLACEMENT_3D('',#33572,#21467,#21468);
#18500=AXIS2_PLACEMENT_3D('',#33573,#21469,#21470);
#18501=AXIS2_PLACEMENT_3D('',#33582,#21475,#21476);
#18502=AXIS2_PLACEMENT_3D('',#33596,#21484,#21485);
#18503=AXIS2_PLACEMENT_3D('',#33607,#21490,#21491);
#18504=AXIS2_PLACEMENT_3D('',#33611,#21494,#21495);
#18505=AXIS2_PLACEMENT_3D('',#33622,#21500,#21501);
#18506=AXIS2_PLACEMENT_3D('',#33630,#21506,#21507);
#18507=AXIS2_PLACEMENT_3D('',#33635,#21509,#21510);
#18508=AXIS2_PLACEMENT_3D('',#33638,#21512,#21513);
#18509=AXIS2_PLACEMENT_3D('',#33639,#21514,#21515);
#18510=AXIS2_PLACEMENT_3D('',#33648,#21516,#21517);
#18511=AXIS2_PLACEMENT_3D('',#33660,#21519,#21520);
#18512=AXIS2_PLACEMENT_3D('',#33664,#21522,#21523);
#18513=AXIS2_PLACEMENT_3D('',#33665,#21524,#21525);
#18514=AXIS2_PLACEMENT_3D('',#33666,#21526,#21527);
#18515=AXIS2_PLACEMENT_3D('',#33676,#21529,#21530);
#18516=AXIS2_PLACEMENT_3D('',#33678,#21532,#21533);
#18517=AXIS2_PLACEMENT_3D('',#33679,#21534,#21535);
#18518=AXIS2_PLACEMENT_3D('',#33681,#21537,#21538);
#18519=AXIS2_PLACEMENT_3D('',#33683,#21540,#21541);
#18520=AXIS2_PLACEMENT_3D('',#33692,#21542,#21543);
#18521=AXIS2_PLACEMENT_3D('',#33698,#21546,#21547);
#18522=AXIS2_PLACEMENT_3D('',#33702,#21550,#21551);
#18523=AXIS2_PLACEMENT_3D('',#33706,#21554,#21555);
#18524=AXIS2_PLACEMENT_3D('',#33712,#21559,#21560);
#18525=AXIS2_PLACEMENT_3D('',#33716,#21563,#21564);
#18526=AXIS2_PLACEMENT_3D('',#33717,#21565,#21566);
#18527=AXIS2_PLACEMENT_3D('',#33718,#21567,#21568);
#18528=AXIS2_PLACEMENT_3D('',#33723,#21571,#21572);
#18529=AXIS2_PLACEMENT_3D('',#33724,#21573,#21574);
#18530=AXIS2_PLACEMENT_3D('',#33730,#21578,#21579);
#18531=AXIS2_PLACEMENT_3D('',#33731,#21580,#21581);
#18532=AXIS2_PLACEMENT_3D('',#33732,#21582,#21583);
#18533=AXIS2_PLACEMENT_3D('',#33733,#21584,#21585);
#18534=AXIS2_PLACEMENT_3D('',#33734,#21586,#21587);
#18535=AXIS2_PLACEMENT_3D('',#33735,#21588,#21589);
#18536=AXIS2_PLACEMENT_3D('',#33736,#21590,#21591);
#18537=AXIS2_PLACEMENT_3D('',#33737,#21592,#21593);
#18538=AXIS2_PLACEMENT_3D('',#33738,#21594,#21595);
#18539=AXIS2_PLACEMENT_3D('',#33739,#21596,#21597);
#18540=AXIS2_PLACEMENT_3D('',#33740,#21598,#21599);
#18541=AXIS2_PLACEMENT_3D('',#33741,#21600,#21601);
#18542=AXIS2_PLACEMENT_3D('',#33742,#21602,#21603);
#18543=AXIS2_PLACEMENT_3D('',#33743,#21604,#21605);
#18544=AXIS2_PLACEMENT_3D('',#33744,#21606,#21607);
#18545=AXIS2_PLACEMENT_3D('',#33745,#21608,#21609);
#18546=AXIS2_PLACEMENT_3D('',#33746,#21610,#21611);
#18547=AXIS2_PLACEMENT_3D('',#33747,#21612,#21613);
#18548=AXIS2_PLACEMENT_3D('',#33748,#21614,#21615);
#18549=AXIS2_PLACEMENT_3D('',#33749,#21616,#21617);
#18550=AXIS2_PLACEMENT_3D('',#33750,#21618,#21619);
#18551=AXIS2_PLACEMENT_3D('',#33751,#21620,#21621);
#18552=AXIS2_PLACEMENT_3D('',#33752,#21622,#21623);
#18553=AXIS2_PLACEMENT_3D('',#33753,#21624,#21625);
#18554=AXIS2_PLACEMENT_3D('',#33754,#21626,#21627);
#18555=AXIS2_PLACEMENT_3D('',#33755,#21628,#21629);
#18556=AXIS2_PLACEMENT_3D('',#33756,#21630,#21631);
#18557=AXIS2_PLACEMENT_3D('',#33757,#21632,#21633);
#18558=AXIS2_PLACEMENT_3D('',#33758,#21634,#21635);
#18559=AXIS2_PLACEMENT_3D('',#33759,#21636,#21637);
#18560=AXIS2_PLACEMENT_3D('',#33760,#21638,#21639);
#18561=AXIS2_PLACEMENT_3D('',#33761,#21640,#21641);
#18562=AXIS2_PLACEMENT_3D('',#33762,#21642,#21643);
#18563=AXIS2_PLACEMENT_3D('',#33763,#21644,#21645);
#18564=AXIS2_PLACEMENT_3D('',#33764,#21646,#21647);
#18565=AXIS2_PLACEMENT_3D('',#33765,#21648,#21649);
#18566=AXIS2_PLACEMENT_3D('',#33766,#21650,#21651);
#18567=AXIS2_PLACEMENT_3D('',#33767,#21652,#21653);
#18568=AXIS2_PLACEMENT_3D('',#33768,#21654,#21655);
#18569=AXIS2_PLACEMENT_3D('',#33769,#21656,#21657);
#18570=AXIS2_PLACEMENT_3D('',#33770,#21658,#21659);
#18571=AXIS2_PLACEMENT_3D('',#33771,#21660,#21661);
#18572=AXIS2_PLACEMENT_3D('',#33772,#21662,#21663);
#18573=AXIS2_PLACEMENT_3D('',#33773,#21664,#21665);
#18574=AXIS2_PLACEMENT_3D('',#33774,#21666,#21667);
#18575=AXIS2_PLACEMENT_3D('',#33775,#21668,#21669);
#18576=AXIS2_PLACEMENT_3D('',#33776,#21670,#21671);
#18577=AXIS2_PLACEMENT_3D('',#33777,#21672,#21673);
#18578=AXIS2_PLACEMENT_3D('',#33778,#21674,#21675);
#18579=AXIS2_PLACEMENT_3D('',#33779,#21676,#21677);
#18580=AXIS2_PLACEMENT_3D('',#33780,#21678,#21679);
#18581=AXIS2_PLACEMENT_3D('',#33781,#21680,#21681);
#18582=AXIS2_PLACEMENT_3D('',#33782,#21682,#21683);
#18583=AXIS2_PLACEMENT_3D('',#33783,#21684,#21685);
#18584=AXIS2_PLACEMENT_3D('',#33784,#21686,#21687);
#18585=AXIS2_PLACEMENT_3D('',#33785,#21688,#21689);
#18586=AXIS2_PLACEMENT_3D('',#33786,#21690,#21691);
#18587=AXIS2_PLACEMENT_3D('',#33787,#21692,#21693);
#18588=AXIS2_PLACEMENT_3D('',#33788,#21694,#21695);
#18589=AXIS2_PLACEMENT_3D('',#33789,#21696,#21697);
#18590=AXIS2_PLACEMENT_3D('',#33790,#21698,#21699);
#18591=AXIS2_PLACEMENT_3D('',#33791,#21700,#21701);
#18592=AXIS2_PLACEMENT_3D('',#33792,#21702,#21703);
#18593=AXIS2_PLACEMENT_3D('',#33793,#21704,#21705);
#18594=AXIS2_PLACEMENT_3D('',#33794,#21706,#21707);
#18595=AXIS2_PLACEMENT_3D('',#33795,#21708,#21709);
#18596=AXIS2_PLACEMENT_3D('',#33796,#21710,#21711);
#18597=AXIS2_PLACEMENT_3D('',#33797,#21712,#21713);
#18598=AXIS2_PLACEMENT_3D('',#33799,#21714,#21715);
#18599=AXIS2_PLACEMENT_3D('',#33801,#21716,#21717);
#18600=AXIS2_PLACEMENT_3D('',#33803,#21718,#21719);
#18601=AXIS2_PLACEMENT_3D('',#33804,#21720,#21721);
#18602=AXIS2_PLACEMENT_3D('',#33805,#21722,#21723);
#18603=AXIS2_PLACEMENT_3D('',#33808,#21724,#21725);
#18604=AXIS2_PLACEMENT_3D('',#33809,#21726,#21727);
#18605=AXIS2_PLACEMENT_3D('',#33811,#21728,#21729);
#18606=AXIS2_PLACEMENT_3D('',#33812,#21730,#21731);
#18607=AXIS2_PLACEMENT_3D('',#33813,#21732,#21733);
#18608=AXIS2_PLACEMENT_3D('',#33815,#21735,#21736);
#18609=AXIS2_PLACEMENT_3D('',#33816,#21737,#21738);
#18610=AXIS2_PLACEMENT_3D('',#33817,#21739,#21740);
#18611=AXIS2_PLACEMENT_3D('',#33819,#21741,#21742);
#18612=AXIS2_PLACEMENT_3D('',#33822,#21744,#21745);
#18613=AXIS2_PLACEMENT_3D('',#33823,#21746,#21747);
#18614=AXIS2_PLACEMENT_3D('',#33826,#21748,#21749);
#18615=AXIS2_PLACEMENT_3D('',#33828,#21750,#21751);
#18616=AXIS2_PLACEMENT_3D('',#33831,#21753,#21754);
#18617=AXIS2_PLACEMENT_3D('',#33832,#21755,#21756);
#18618=AXIS2_PLACEMENT_3D('',#33833,#21757,#21758);
#18619=AXIS2_PLACEMENT_3D('',#33835,#21759,#21760);
#18620=AXIS2_PLACEMENT_3D('',#33838,#21762,#21763);
#18621=AXIS2_PLACEMENT_3D('',#33839,#21764,#21765);
#18622=AXIS2_PLACEMENT_3D('',#33841,#21766,#21767);
#18623=AXIS2_PLACEMENT_3D('',#33844,#21769,#21770);
#18624=AXIS2_PLACEMENT_3D('',#33845,#21771,#21772);
#18625=AXIS2_PLACEMENT_3D('',#33847,#21773,#21774);
#18626=AXIS2_PLACEMENT_3D('',#33850,#21776,#21777);
#18627=AXIS2_PLACEMENT_3D('',#33851,#21778,#21779);
#18628=AXIS2_PLACEMENT_3D('',#33853,#21780,#21781);
#18629=AXIS2_PLACEMENT_3D('',#33856,#21783,#21784);
#18630=AXIS2_PLACEMENT_3D('',#33857,#21785,#21786);
#18631=AXIS2_PLACEMENT_3D('',#33863,#21790,#21791);
#18632=AXIS2_PLACEMENT_3D('',#33868,#21793,#21794);
#18633=AXIS2_PLACEMENT_3D('',#33871,#21796,#21797);
#18634=AXIS2_PLACEMENT_3D('',#33872,#21798,#21799);
#18635=AXIS2_PLACEMENT_3D('',#33878,#21803,#21804);
#18636=AXIS2_PLACEMENT_3D('',#33881,#21807,#21808);
#18637=AXIS2_PLACEMENT_3D('',#33890,#21812,#21813);
#18638=AXIS2_PLACEMENT_3D('',#33892,#21815,#21816);
#18639=AXIS2_PLACEMENT_3D('',#33895,#21819,#21820);
#18640=AXIS2_PLACEMENT_3D('',#33903,#21825,#21826);
#18641=AXIS2_PLACEMENT_3D('',#33906,#21828,#21829);
#18642=AXIS2_PLACEMENT_3D('',#33907,#21830,#21831);
#18643=AXIS2_PLACEMENT_3D('',#33911,#21834,#21835);
#18644=AXIS2_PLACEMENT_3D('',#33917,#21839,#21840);
#18645=AXIS2_PLACEMENT_3D('',#33919,#21842,#21843);
#18646=AXIS2_PLACEMENT_3D('',#33921,#21845,#21846);
#18647=AXIS2_PLACEMENT_3D('',#33922,#21847,#21848);
#18648=AXIS2_PLACEMENT_3D('',#33923,#21849,#21850);
#18649=AXIS2_PLACEMENT_3D('',#33924,#21851,#21852);
#18650=AXIS2_PLACEMENT_3D('',#33925,#21853,#21854);
#18651=AXIS2_PLACEMENT_3D('',#33927,#21855,#21856);
#18652=AXIS2_PLACEMENT_3D('',#33930,#21858,#21859);
#18653=AXIS2_PLACEMENT_3D('',#33931,#21860,#21861);
#18654=AXIS2_PLACEMENT_3D('',#33934,#21862,#21863);
#18655=AXIS2_PLACEMENT_3D('',#33935,#21864,#21865);
#18656=AXIS2_PLACEMENT_3D('',#33936,#21866,#21867);
#18657=AXIS2_PLACEMENT_3D('',#33938,#21868,#21869);
#18658=AXIS2_PLACEMENT_3D('',#33940,#21870,#21871);
#18659=AXIS2_PLACEMENT_3D('',#33941,#21872,#21873);
#18660=AXIS2_PLACEMENT_3D('',#33942,#21874,#21875);
#18661=AXIS2_PLACEMENT_3D('',#33945,#21876,#21877);
#18662=AXIS2_PLACEMENT_3D('',#33946,#21878,#21879);
#18663=AXIS2_PLACEMENT_3D('',#33949,#21881,#21882);
#18664=AXIS2_PLACEMENT_3D('',#33950,#21883,#21884);
#18665=AXIS2_PLACEMENT_3D('',#33953,#21885,#21886);
#18666=AXIS2_PLACEMENT_3D('',#33954,#21887,#21888);
#18667=AXIS2_PLACEMENT_3D('',#33958,#21890,#21891);
#18668=AXIS2_PLACEMENT_3D('',#33959,#21892,#21893);
#18669=AXIS2_PLACEMENT_3D('',#33960,#21894,#21895);
#18670=AXIS2_PLACEMENT_3D('',#33962,#21897,#21898);
#18671=AXIS2_PLACEMENT_3D('',#33965,#21899,#21900);
#18672=AXIS2_PLACEMENT_3D('',#33966,#21901,#21902);
#18673=AXIS2_PLACEMENT_3D('',#33968,#21904,#21905);
#18674=AXIS2_PLACEMENT_3D('',#33971,#21906,#21907);
#18675=AXIS2_PLACEMENT_3D('',#33972,#21908,#21909);
#18676=AXIS2_PLACEMENT_3D('',#33976,#21911,#21912);
#18677=AXIS2_PLACEMENT_3D('',#33977,#21913,#21914);
#18678=AXIS2_PLACEMENT_3D('',#33978,#21915,#21916);
#18679=AXIS2_PLACEMENT_3D('',#33980,#21918,#21919);
#18680=AXIS2_PLACEMENT_3D('',#33983,#21920,#21921);
#18681=AXIS2_PLACEMENT_3D('',#33984,#21922,#21923);
#18682=AXIS2_PLACEMENT_3D('',#33986,#21925,#21926);
#18683=AXIS2_PLACEMENT_3D('',#33989,#21927,#21928);
#18684=AXIS2_PLACEMENT_3D('',#33990,#21929,#21930);
#18685=AXIS2_PLACEMENT_3D('',#33994,#21932,#21933);
#18686=AXIS2_PLACEMENT_3D('',#33995,#21934,#21935);
#18687=AXIS2_PLACEMENT_3D('',#33996,#21936,#21937);
#18688=AXIS2_PLACEMENT_3D('',#33998,#21939,#21940);
#18689=AXIS2_PLACEMENT_3D('',#34001,#21941,#21942);
#18690=AXIS2_PLACEMENT_3D('',#34002,#21943,#21944);
#18691=AXIS2_PLACEMENT_3D('',#34004,#21946,#21947);
#18692=AXIS2_PLACEMENT_3D('',#34007,#21948,#21949);
#18693=AXIS2_PLACEMENT_3D('',#34008,#21950,#21951);
#18694=AXIS2_PLACEMENT_3D('',#34012,#21953,#21954);
#18695=AXIS2_PLACEMENT_3D('',#34013,#21955,#21956);
#18696=AXIS2_PLACEMENT_3D('',#34014,#21957,#21958);
#18697=AXIS2_PLACEMENT_3D('',#34016,#21960,#21961);
#18698=AXIS2_PLACEMENT_3D('',#34019,#21962,#21963);
#18699=AXIS2_PLACEMENT_3D('',#34020,#21964,#21965);
#18700=AXIS2_PLACEMENT_3D('',#34022,#21967,#21968);
#18701=AXIS2_PLACEMENT_3D('',#34025,#21969,#21970);
#18702=AXIS2_PLACEMENT_3D('',#34026,#21971,#21972);
#18703=AXIS2_PLACEMENT_3D('',#34030,#21974,#21975);
#18704=AXIS2_PLACEMENT_3D('',#34031,#21976,#21977);
#18705=AXIS2_PLACEMENT_3D('',#34032,#21978,#21979);
#18706=AXIS2_PLACEMENT_3D('',#34034,#21981,#21982);
#18707=AXIS2_PLACEMENT_3D('',#34037,#21983,#21984);
#18708=AXIS2_PLACEMENT_3D('',#34038,#21985,#21986);
#18709=AXIS2_PLACEMENT_3D('',#34040,#21988,#21989);
#18710=AXIS2_PLACEMENT_3D('',#34043,#21990,#21991);
#18711=AXIS2_PLACEMENT_3D('',#34044,#21992,#21993);
#18712=AXIS2_PLACEMENT_3D('',#34048,#21995,#21996);
#18713=AXIS2_PLACEMENT_3D('',#34049,#21997,#21998);
#18714=AXIS2_PLACEMENT_3D('',#34050,#21999,#22000);
#18715=AXIS2_PLACEMENT_3D('',#34052,#22002,#22003);
#18716=AXIS2_PLACEMENT_3D('',#34055,#22004,#22005);
#18717=AXIS2_PLACEMENT_3D('',#34056,#22006,#22007);
#18718=AXIS2_PLACEMENT_3D('',#34058,#22009,#22010);
#18719=AXIS2_PLACEMENT_3D('',#34061,#22011,#22012);
#18720=AXIS2_PLACEMENT_3D('',#34062,#22013,#22014);
#18721=AXIS2_PLACEMENT_3D('',#34066,#22016,#22017);
#18722=AXIS2_PLACEMENT_3D('',#34067,#22018,#22019);
#18723=AXIS2_PLACEMENT_3D('',#34068,#22020,#22021);
#18724=AXIS2_PLACEMENT_3D('',#34070,#22023,#22024);
#18725=AXIS2_PLACEMENT_3D('',#34073,#22025,#22026);
#18726=AXIS2_PLACEMENT_3D('',#34074,#22027,#22028);
#18727=AXIS2_PLACEMENT_3D('',#34076,#22030,#22031);
#18728=AXIS2_PLACEMENT_3D('',#34079,#22032,#22033);
#18729=AXIS2_PLACEMENT_3D('',#34080,#22034,#22035);
#18730=AXIS2_PLACEMENT_3D('',#34084,#22037,#22038);
#18731=AXIS2_PLACEMENT_3D('',#34085,#22039,#22040);
#18732=AXIS2_PLACEMENT_3D('',#34086,#22041,#22042);
#18733=AXIS2_PLACEMENT_3D('',#34088,#22044,#22045);
#18734=AXIS2_PLACEMENT_3D('',#34091,#22046,#22047);
#18735=AXIS2_PLACEMENT_3D('',#34092,#22048,#22049);
#18736=AXIS2_PLACEMENT_3D('',#34094,#22051,#22052);
#18737=AXIS2_PLACEMENT_3D('',#34097,#22053,#22054);
#18738=AXIS2_PLACEMENT_3D('',#34098,#22055,#22056);
#18739=AXIS2_PLACEMENT_3D('',#34102,#22058,#22059);
#18740=AXIS2_PLACEMENT_3D('',#34103,#22060,#22061);
#18741=AXIS2_PLACEMENT_3D('',#34104,#22062,#22063);
#18742=AXIS2_PLACEMENT_3D('',#34106,#22065,#22066);
#18743=AXIS2_PLACEMENT_3D('',#34109,#22067,#22068);
#18744=AXIS2_PLACEMENT_3D('',#34110,#22069,#22070);
#18745=AXIS2_PLACEMENT_3D('',#34112,#22072,#22073);
#18746=AXIS2_PLACEMENT_3D('',#34115,#22074,#22075);
#18747=AXIS2_PLACEMENT_3D('',#34116,#22076,#22077);
#18748=AXIS2_PLACEMENT_3D('',#34120,#22079,#22080);
#18749=AXIS2_PLACEMENT_3D('',#34121,#22081,#22082);
#18750=AXIS2_PLACEMENT_3D('',#34122,#22083,#22084);
#18751=AXIS2_PLACEMENT_3D('',#34124,#22086,#22087);
#18752=AXIS2_PLACEMENT_3D('',#34127,#22088,#22089);
#18753=AXIS2_PLACEMENT_3D('',#34128,#22090,#22091);
#18754=AXIS2_PLACEMENT_3D('',#34130,#22093,#22094);
#18755=AXIS2_PLACEMENT_3D('',#34133,#22095,#22096);
#18756=AXIS2_PLACEMENT_3D('',#34134,#22097,#22098);
#18757=AXIS2_PLACEMENT_3D('',#34138,#22100,#22101);
#18758=AXIS2_PLACEMENT_3D('',#34139,#22102,#22103);
#18759=AXIS2_PLACEMENT_3D('',#34140,#22104,#22105);
#18760=AXIS2_PLACEMENT_3D('',#34142,#22107,#22108);
#18761=AXIS2_PLACEMENT_3D('',#34145,#22109,#22110);
#18762=AXIS2_PLACEMENT_3D('',#34146,#22111,#22112);
#18763=AXIS2_PLACEMENT_3D('',#34148,#22114,#22115);
#18764=AXIS2_PLACEMENT_3D('',#34151,#22116,#22117);
#18765=AXIS2_PLACEMENT_3D('',#34152,#22118,#22119);
#18766=AXIS2_PLACEMENT_3D('',#34156,#22121,#22122);
#18767=AXIS2_PLACEMENT_3D('',#34157,#22123,#22124);
#18768=AXIS2_PLACEMENT_3D('',#34158,#22125,#22126);
#18769=AXIS2_PLACEMENT_3D('',#34160,#22128,#22129);
#18770=AXIS2_PLACEMENT_3D('',#34163,#22130,#22131);
#18771=AXIS2_PLACEMENT_3D('',#34164,#22132,#22133);
#18772=AXIS2_PLACEMENT_3D('',#34166,#22135,#22136);
#18773=AXIS2_PLACEMENT_3D('',#34169,#22137,#22138);
#18774=AXIS2_PLACEMENT_3D('',#34170,#22139,#22140);
#18775=AXIS2_PLACEMENT_3D('',#34174,#22142,#22143);
#18776=AXIS2_PLACEMENT_3D('',#34175,#22144,#22145);
#18777=AXIS2_PLACEMENT_3D('',#34176,#22146,#22147);
#18778=AXIS2_PLACEMENT_3D('',#34178,#22149,#22150);
#18779=AXIS2_PLACEMENT_3D('',#34181,#22151,#22152);
#18780=AXIS2_PLACEMENT_3D('',#34182,#22153,#22154);
#18781=AXIS2_PLACEMENT_3D('',#34184,#22156,#22157);
#18782=AXIS2_PLACEMENT_3D('',#34187,#22158,#22159);
#18783=AXIS2_PLACEMENT_3D('',#34188,#22160,#22161);
#18784=AXIS2_PLACEMENT_3D('',#34192,#22163,#22164);
#18785=AXIS2_PLACEMENT_3D('',#34193,#22165,#22166);
#18786=AXIS2_PLACEMENT_3D('',#34194,#22167,#22168);
#18787=AXIS2_PLACEMENT_3D('',#34196,#22170,#22171);
#18788=AXIS2_PLACEMENT_3D('',#34199,#22172,#22173);
#18789=AXIS2_PLACEMENT_3D('',#34200,#22174,#22175);
#18790=AXIS2_PLACEMENT_3D('',#34202,#22177,#22178);
#18791=AXIS2_PLACEMENT_3D('',#34205,#22179,#22180);
#18792=AXIS2_PLACEMENT_3D('',#34206,#22181,#22182);
#18793=AXIS2_PLACEMENT_3D('',#34210,#22184,#22185);
#18794=AXIS2_PLACEMENT_3D('',#34211,#22186,#22187);
#18795=AXIS2_PLACEMENT_3D('',#34212,#22188,#22189);
#18796=AXIS2_PLACEMENT_3D('',#34214,#22191,#22192);
#18797=AXIS2_PLACEMENT_3D('',#34221,#22193,#22194);
#18798=AXIS2_PLACEMENT_3D('',#34231,#22195,#22196);
#18799=AXIS2_PLACEMENT_3D('',#34241,#22197,#22198);
#18800=AXIS2_PLACEMENT_3D('',#34251,#22199,#22200);
#18801=AXIS2_PLACEMENT_3D('',#34261,#22201,#22202);
#18802=AXIS2_PLACEMENT_3D('',#34271,#22203,#22204);
#18803=AXIS2_PLACEMENT_3D('',#34281,#22205,#22206);
#18804=AXIS2_PLACEMENT_3D('',#34291,#22207,#22208);
#18805=AXIS2_PLACEMENT_3D('',#34301,#22209,#22210);
#18806=AXIS2_PLACEMENT_3D('',#34311,#22211,#22212);
#18807=AXIS2_PLACEMENT_3D('',#34321,#22213,#22214);
#18808=AXIS2_PLACEMENT_3D('',#34331,#22215,#22216);
#18809=AXIS2_PLACEMENT_3D('',#34341,#22217,#22218);
#18810=AXIS2_PLACEMENT_3D('',#34351,#22219,#22220);
#18811=AXIS2_PLACEMENT_3D('',#34361,#22221,#22222);
#18812=AXIS2_PLACEMENT_3D('',#34371,#22223,#22224);
#18813=AXIS2_PLACEMENT_3D('',#34381,#22225,#22226);
#18814=AXIS2_PLACEMENT_3D('',#34391,#22227,#22228);
#18815=AXIS2_PLACEMENT_3D('',#34401,#22229,#22230);
#18816=AXIS2_PLACEMENT_3D('',#34411,#22231,#22232);
#18817=AXIS2_PLACEMENT_3D('',#34421,#22233,#22234);
#18818=AXIS2_PLACEMENT_3D('',#34431,#22235,#22236);
#18819=AXIS2_PLACEMENT_3D('',#34441,#22237,#22238);
#18820=AXIS2_PLACEMENT_3D('',#34451,#22239,#22240);
#18821=AXIS2_PLACEMENT_3D('',#34461,#22241,#22242);
#18822=AXIS2_PLACEMENT_3D('',#34471,#22243,#22244);
#18823=AXIS2_PLACEMENT_3D('',#34481,#22245,#22246);
#18824=AXIS2_PLACEMENT_3D('',#34491,#22247,#22248);
#18825=AXIS2_PLACEMENT_3D('',#34501,#22249,#22250);
#18826=AXIS2_PLACEMENT_3D('',#34511,#22251,#22252);
#18827=AXIS2_PLACEMENT_3D('',#34521,#22253,#22254);
#18828=AXIS2_PLACEMENT_3D('',#34531,#22255,#22256);
#18829=AXIS2_PLACEMENT_3D('',#34541,#22257,#22258);
#18830=AXIS2_PLACEMENT_3D('',#34551,#22259,#22260);
#18831=AXIS2_PLACEMENT_3D('',#34561,#22261,#22262);
#18832=AXIS2_PLACEMENT_3D('',#34571,#22263,#22264);
#18833=AXIS2_PLACEMENT_3D('',#34581,#22265,#22266);
#18834=AXIS2_PLACEMENT_3D('',#34591,#22267,#22268);
#18835=AXIS2_PLACEMENT_3D('',#34601,#22269,#22270);
#18836=AXIS2_PLACEMENT_3D('',#34608,#22272,#22273);
#18837=AXIS2_PLACEMENT_3D('',#34618,#22274,#22275);
#18838=AXIS2_PLACEMENT_3D('',#34628,#22276,#22277);
#18839=AXIS2_PLACEMENT_3D('',#34638,#22278,#22279);
#18840=AXIS2_PLACEMENT_3D('',#34648,#22280,#22281);
#18841=AXIS2_PLACEMENT_3D('',#34658,#22282,#22283);
#18842=AXIS2_PLACEMENT_3D('',#34668,#22284,#22285);
#18843=AXIS2_PLACEMENT_3D('',#34678,#22286,#22287);
#18844=AXIS2_PLACEMENT_3D('',#34688,#22288,#22289);
#18845=AXIS2_PLACEMENT_3D('',#34698,#22290,#22291);
#18846=AXIS2_PLACEMENT_3D('',#34708,#22292,#22293);
#18847=AXIS2_PLACEMENT_3D('',#34718,#22294,#22295);
#18848=AXIS2_PLACEMENT_3D('',#34728,#22296,#22297);
#18849=AXIS2_PLACEMENT_3D('',#34738,#22298,#22299);
#18850=AXIS2_PLACEMENT_3D('',#34748,#22300,#22301);
#18851=AXIS2_PLACEMENT_3D('',#34758,#22302,#22303);
#18852=AXIS2_PLACEMENT_3D('',#34768,#22304,#22305);
#18853=AXIS2_PLACEMENT_3D('',#34778,#22306,#22307);
#18854=AXIS2_PLACEMENT_3D('',#34788,#22308,#22309);
#18855=AXIS2_PLACEMENT_3D('',#34798,#22310,#22311);
#18856=AXIS2_PLACEMENT_3D('',#34808,#22312,#22313);
#18857=AXIS2_PLACEMENT_3D('',#34818,#22314,#22315);
#18858=AXIS2_PLACEMENT_3D('',#34828,#22316,#22317);
#18859=AXIS2_PLACEMENT_3D('',#34838,#22318,#22319);
#18860=AXIS2_PLACEMENT_3D('',#34848,#22320,#22321);
#18861=AXIS2_PLACEMENT_3D('',#34858,#22322,#22323);
#18862=AXIS2_PLACEMENT_3D('',#34868,#22324,#22325);
#18863=AXIS2_PLACEMENT_3D('',#34878,#22326,#22327);
#18864=AXIS2_PLACEMENT_3D('',#34888,#22328,#22329);
#18865=AXIS2_PLACEMENT_3D('',#34898,#22330,#22331);
#18866=AXIS2_PLACEMENT_3D('',#34908,#22332,#22333);
#18867=AXIS2_PLACEMENT_3D('',#34918,#22334,#22335);
#18868=AXIS2_PLACEMENT_3D('',#34928,#22336,#22337);
#18869=AXIS2_PLACEMENT_3D('',#34938,#22338,#22339);
#18870=AXIS2_PLACEMENT_3D('',#34948,#22340,#22341);
#18871=AXIS2_PLACEMENT_3D('',#34958,#22342,#22343);
#18872=AXIS2_PLACEMENT_3D('',#34968,#22344,#22345);
#18873=AXIS2_PLACEMENT_3D('',#34978,#22346,#22347);
#18874=AXIS2_PLACEMENT_3D('',#34988,#22348,#22349);
#18875=AXIS2_PLACEMENT_3D('',#34992,#22350,#22351);
#18876=AXIS2_PLACEMENT_3D('',#34999,#22352,#22353);
#18877=AXIS2_PLACEMENT_3D('',#35009,#22354,#22355);
#18878=AXIS2_PLACEMENT_3D('',#35019,#22356,#22357);
#18879=AXIS2_PLACEMENT_3D('',#35029,#22358,#22359);
#18880=AXIS2_PLACEMENT_3D('',#35039,#22360,#22361);
#18881=AXIS2_PLACEMENT_3D('',#35049,#22362,#22363);
#18882=AXIS2_PLACEMENT_3D('',#35059,#22364,#22365);
#18883=AXIS2_PLACEMENT_3D('',#35069,#22366,#22367);
#18884=AXIS2_PLACEMENT_3D('',#35079,#22368,#22369);
#18885=AXIS2_PLACEMENT_3D('',#35089,#22370,#22371);
#18886=AXIS2_PLACEMENT_3D('',#35099,#22372,#22373);
#18887=AXIS2_PLACEMENT_3D('',#35109,#22374,#22375);
#18888=AXIS2_PLACEMENT_3D('',#35119,#22376,#22377);
#18889=AXIS2_PLACEMENT_3D('',#35129,#22378,#22379);
#18890=AXIS2_PLACEMENT_3D('',#35139,#22380,#22381);
#18891=AXIS2_PLACEMENT_3D('',#35149,#22382,#22383);
#18892=AXIS2_PLACEMENT_3D('',#35159,#22384,#22385);
#18893=AXIS2_PLACEMENT_3D('',#35169,#22386,#22387);
#18894=AXIS2_PLACEMENT_3D('',#35179,#22388,#22389);
#18895=AXIS2_PLACEMENT_3D('',#35189,#22390,#22391);
#18896=AXIS2_PLACEMENT_3D('',#35199,#22392,#22393);
#18897=AXIS2_PLACEMENT_3D('',#35209,#22394,#22395);
#18898=AXIS2_PLACEMENT_3D('',#35219,#22396,#22397);
#18899=AXIS2_PLACEMENT_3D('',#35229,#22398,#22399);
#18900=AXIS2_PLACEMENT_3D('',#35239,#22400,#22401);
#18901=AXIS2_PLACEMENT_3D('',#35249,#22402,#22403);
#18902=AXIS2_PLACEMENT_3D('',#35259,#22404,#22405);
#18903=AXIS2_PLACEMENT_3D('',#35269,#22406,#22407);
#18904=AXIS2_PLACEMENT_3D('',#35279,#22408,#22409);
#18905=AXIS2_PLACEMENT_3D('',#35289,#22410,#22411);
#18906=AXIS2_PLACEMENT_3D('',#35299,#22412,#22413);
#18907=AXIS2_PLACEMENT_3D('',#35309,#22414,#22415);
#18908=AXIS2_PLACEMENT_3D('',#35319,#22416,#22417);
#18909=AXIS2_PLACEMENT_3D('',#35329,#22418,#22419);
#18910=AXIS2_PLACEMENT_3D('',#35339,#22420,#22421);
#18911=AXIS2_PLACEMENT_3D('',#35349,#22422,#22423);
#18912=AXIS2_PLACEMENT_3D('',#35359,#22424,#22425);
#18913=AXIS2_PLACEMENT_3D('',#35369,#22426,#22427);
#18914=AXIS2_PLACEMENT_3D('',#35379,#22428,#22429);
#18915=AXIS2_PLACEMENT_3D('',#35386,#22431,#22432);
#18916=AXIS2_PLACEMENT_3D('',#35396,#22433,#22434);
#18917=AXIS2_PLACEMENT_3D('',#35406,#22435,#22436);
#18918=AXIS2_PLACEMENT_3D('',#35416,#22437,#22438);
#18919=AXIS2_PLACEMENT_3D('',#35426,#22439,#22440);
#18920=AXIS2_PLACEMENT_3D('',#35436,#22441,#22442);
#18921=AXIS2_PLACEMENT_3D('',#35446,#22443,#22444);
#18922=AXIS2_PLACEMENT_3D('',#35456,#22445,#22446);
#18923=AXIS2_PLACEMENT_3D('',#35466,#22447,#22448);
#18924=AXIS2_PLACEMENT_3D('',#35476,#22449,#22450);
#18925=AXIS2_PLACEMENT_3D('',#35486,#22451,#22452);
#18926=AXIS2_PLACEMENT_3D('',#35496,#22453,#22454);
#18927=AXIS2_PLACEMENT_3D('',#35506,#22455,#22456);
#18928=AXIS2_PLACEMENT_3D('',#35516,#22457,#22458);
#18929=AXIS2_PLACEMENT_3D('',#35526,#22459,#22460);
#18930=AXIS2_PLACEMENT_3D('',#35536,#22461,#22462);
#18931=AXIS2_PLACEMENT_3D('',#35546,#22463,#22464);
#18932=AXIS2_PLACEMENT_3D('',#35556,#22465,#22466);
#18933=AXIS2_PLACEMENT_3D('',#35566,#22467,#22468);
#18934=AXIS2_PLACEMENT_3D('',#35576,#22469,#22470);
#18935=AXIS2_PLACEMENT_3D('',#35586,#22471,#22472);
#18936=AXIS2_PLACEMENT_3D('',#35596,#22473,#22474);
#18937=AXIS2_PLACEMENT_3D('',#35606,#22475,#22476);
#18938=AXIS2_PLACEMENT_3D('',#35616,#22477,#22478);
#18939=AXIS2_PLACEMENT_3D('',#35626,#22479,#22480);
#18940=AXIS2_PLACEMENT_3D('',#35636,#22481,#22482);
#18941=AXIS2_PLACEMENT_3D('',#35646,#22483,#22484);
#18942=AXIS2_PLACEMENT_3D('',#35656,#22485,#22486);
#18943=AXIS2_PLACEMENT_3D('',#35666,#22487,#22488);
#18944=AXIS2_PLACEMENT_3D('',#35676,#22489,#22490);
#18945=AXIS2_PLACEMENT_3D('',#35686,#22491,#22492);
#18946=AXIS2_PLACEMENT_3D('',#35696,#22493,#22494);
#18947=AXIS2_PLACEMENT_3D('',#35706,#22495,#22496);
#18948=AXIS2_PLACEMENT_3D('',#35716,#22497,#22498);
#18949=AXIS2_PLACEMENT_3D('',#35726,#22499,#22500);
#18950=AXIS2_PLACEMENT_3D('',#35736,#22501,#22502);
#18951=AXIS2_PLACEMENT_3D('',#35746,#22503,#22504);
#18952=AXIS2_PLACEMENT_3D('',#35756,#22505,#22506);
#18953=AXIS2_PLACEMENT_3D('',#35766,#22507,#22508);
#18954=AXIS2_PLACEMENT_3D('',#35770,#22509,#22510);
#18955=AXIS2_PLACEMENT_3D('',#35772,#22512,#22513);
#18956=AXIS2_PLACEMENT_3D('',#35775,#22516,#22517);
#18957=AXIS2_PLACEMENT_3D('',#35778,#22520,#22521);
#18958=AXIS2_PLACEMENT_3D('',#35781,#22524,#22525);
#18959=AXIS2_PLACEMENT_3D('',#35784,#22528,#22529);
#18960=AXIS2_PLACEMENT_3D('',#35787,#22532,#22533);
#18961=AXIS2_PLACEMENT_3D('',#35790,#22536,#22537);
#18962=AXIS2_PLACEMENT_3D('',#35793,#22540,#22541);
#18963=AXIS2_PLACEMENT_3D('',#35796,#22544,#22545);
#18964=AXIS2_PLACEMENT_3D('',#35799,#22548,#22549);
#18965=AXIS2_PLACEMENT_3D('',#35802,#22552,#22553);
#18966=AXIS2_PLACEMENT_3D('',#35805,#22556,#22557);
#18967=AXIS2_PLACEMENT_3D('',#35808,#22560,#22561);
#18968=AXIS2_PLACEMENT_3D('',#35811,#22564,#22565);
#18969=AXIS2_PLACEMENT_3D('',#35814,#22568,#22569);
#18970=AXIS2_PLACEMENT_3D('',#35817,#22572,#22573);
#18971=AXIS2_PLACEMENT_3D('',#35820,#22576,#22577);
#18972=AXIS2_PLACEMENT_3D('',#35823,#22580,#22581);
#18973=AXIS2_PLACEMENT_3D('',#35826,#22584,#22585);
#18974=AXIS2_PLACEMENT_3D('',#35829,#22588,#22589);
#18975=AXIS2_PLACEMENT_3D('',#35832,#22592,#22593);
#18976=AXIS2_PLACEMENT_3D('',#35835,#22596,#22597);
#18977=AXIS2_PLACEMENT_3D('',#35838,#22600,#22601);
#18978=AXIS2_PLACEMENT_3D('',#35841,#22604,#22605);
#18979=AXIS2_PLACEMENT_3D('',#35844,#22608,#22609);
#18980=AXIS2_PLACEMENT_3D('',#35847,#22612,#22613);
#18981=AXIS2_PLACEMENT_3D('',#35850,#22616,#22617);
#18982=AXIS2_PLACEMENT_3D('',#35853,#22620,#22621);
#18983=AXIS2_PLACEMENT_3D('',#35856,#22624,#22625);
#18984=AXIS2_PLACEMENT_3D('',#35859,#22628,#22629);
#18985=AXIS2_PLACEMENT_3D('',#35862,#22632,#22633);
#18986=AXIS2_PLACEMENT_3D('',#35865,#22636,#22637);
#18987=AXIS2_PLACEMENT_3D('',#35868,#22640,#22641);
#18988=AXIS2_PLACEMENT_3D('',#35871,#22644,#22645);
#18989=AXIS2_PLACEMENT_3D('',#35874,#22648,#22649);
#18990=AXIS2_PLACEMENT_3D('',#35877,#22652,#22653);
#18991=AXIS2_PLACEMENT_3D('',#35880,#22656,#22657);
#18992=AXIS2_PLACEMENT_3D('',#35883,#22660,#22661);
#18993=AXIS2_PLACEMENT_3D('',#35886,#22664,#22665);
#18994=AXIS2_PLACEMENT_3D('',#35889,#22668,#22669);
#18995=AXIS2_PLACEMENT_3D('',#35892,#22672,#22673);
#18996=AXIS2_PLACEMENT_3D('',#35895,#22676,#22677);
#18997=AXIS2_PLACEMENT_3D('',#35898,#22680,#22681);
#18998=AXIS2_PLACEMENT_3D('',#35901,#22684,#22685);
#18999=AXIS2_PLACEMENT_3D('',#35904,#22688,#22689);
#19000=AXIS2_PLACEMENT_3D('',#35907,#22692,#22693);
#19001=AXIS2_PLACEMENT_3D('',#35910,#22696,#22697);
#19002=AXIS2_PLACEMENT_3D('',#35913,#22700,#22701);
#19003=AXIS2_PLACEMENT_3D('',#35916,#22704,#22705);
#19004=AXIS2_PLACEMENT_3D('',#35919,#22708,#22709);
#19005=AXIS2_PLACEMENT_3D('',#35922,#22712,#22713);
#19006=AXIS2_PLACEMENT_3D('',#35925,#22716,#22717);
#19007=AXIS2_PLACEMENT_3D('',#35928,#22720,#22721);
#19008=AXIS2_PLACEMENT_3D('',#35931,#22724,#22725);
#19009=AXIS2_PLACEMENT_3D('',#35934,#22728,#22729);
#19010=AXIS2_PLACEMENT_3D('',#35937,#22732,#22733);
#19011=AXIS2_PLACEMENT_3D('',#35940,#22736,#22737);
#19012=AXIS2_PLACEMENT_3D('',#35943,#22740,#22741);
#19013=AXIS2_PLACEMENT_3D('',#35946,#22744,#22745);
#19014=AXIS2_PLACEMENT_3D('',#35949,#22748,#22749);
#19015=AXIS2_PLACEMENT_3D('',#35952,#22752,#22753);
#19016=AXIS2_PLACEMENT_3D('',#35955,#22756,#22757);
#19017=AXIS2_PLACEMENT_3D('',#35958,#22760,#22761);
#19018=AXIS2_PLACEMENT_3D('',#35961,#22764,#22765);
#19019=AXIS2_PLACEMENT_3D('',#35964,#22768,#22769);
#19020=AXIS2_PLACEMENT_3D('',#35967,#22772,#22773);
#19021=AXIS2_PLACEMENT_3D('',#35970,#22776,#22777);
#19022=AXIS2_PLACEMENT_3D('',#35973,#22780,#22781);
#19023=AXIS2_PLACEMENT_3D('',#35976,#22784,#22785);
#19024=AXIS2_PLACEMENT_3D('',#35979,#22788,#22789);
#19025=AXIS2_PLACEMENT_3D('',#35982,#22792,#22793);
#19026=AXIS2_PLACEMENT_3D('',#35985,#22796,#22797);
#19027=AXIS2_PLACEMENT_3D('',#35988,#22800,#22801);
#19028=AXIS2_PLACEMENT_3D('',#35991,#22804,#22805);
#19029=AXIS2_PLACEMENT_3D('',#35994,#22808,#22809);
#19030=AXIS2_PLACEMENT_3D('',#35997,#22812,#22813);
#19031=AXIS2_PLACEMENT_3D('',#36000,#22816,#22817);
#19032=AXIS2_PLACEMENT_3D('',#36001,#22818,#22819);
#19033=AXIS2_PLACEMENT_3D('',#36004,#22822,#22823);
#19034=AXIS2_PLACEMENT_3D('',#36005,#22824,#22825);
#19035=AXIS2_PLACEMENT_3D('',#36006,#22826,#22827);
#19036=AXIS2_PLACEMENT_3D('',#36008,#22829,#22830);
#19037=AXIS2_PLACEMENT_3D('',#36009,#22831,#22832);
#19038=AXIS2_PLACEMENT_3D('',#36011,#22834,#22835);
#19039=AXIS2_PLACEMENT_3D('',#36012,#22836,#22837);
#19040=AXIS2_PLACEMENT_3D('',#36014,#22839,#22840);
#19041=AXIS2_PLACEMENT_3D('',#36015,#22841,#22842);
#19042=AXIS2_PLACEMENT_3D('',#36017,#22844,#22845);
#19043=AXIS2_PLACEMENT_3D('',#36018,#22846,#22847);
#19044=AXIS2_PLACEMENT_3D('',#36020,#22849,#22850);
#19045=AXIS2_PLACEMENT_3D('',#36021,#22851,#22852);
#19046=AXIS2_PLACEMENT_3D('',#36023,#22854,#22855);
#19047=AXIS2_PLACEMENT_3D('',#36024,#22856,#22857);
#19048=AXIS2_PLACEMENT_3D('',#36026,#22859,#22860);
#19049=AXIS2_PLACEMENT_3D('',#36027,#22861,#22862);
#19050=AXIS2_PLACEMENT_3D('',#36029,#22864,#22865);
#19051=AXIS2_PLACEMENT_3D('',#36030,#22866,#22867);
#19052=AXIS2_PLACEMENT_3D('',#36032,#22869,#22870);
#19053=AXIS2_PLACEMENT_3D('',#36033,#22871,#22872);
#19054=AXIS2_PLACEMENT_3D('',#36035,#22874,#22875);
#19055=AXIS2_PLACEMENT_3D('',#36036,#22876,#22877);
#19056=AXIS2_PLACEMENT_3D('',#36038,#22879,#22880);
#19057=AXIS2_PLACEMENT_3D('',#36039,#22881,#22882);
#19058=AXIS2_PLACEMENT_3D('',#36041,#22884,#22885);
#19059=AXIS2_PLACEMENT_3D('',#36042,#22886,#22887);
#19060=AXIS2_PLACEMENT_3D('',#36044,#22889,#22890);
#19061=AXIS2_PLACEMENT_3D('',#36045,#22891,#22892);
#19062=AXIS2_PLACEMENT_3D('',#36047,#22894,#22895);
#19063=AXIS2_PLACEMENT_3D('',#36048,#22896,#22897);
#19064=AXIS2_PLACEMENT_3D('',#36050,#22899,#22900);
#19065=AXIS2_PLACEMENT_3D('',#36051,#22901,#22902);
#19066=AXIS2_PLACEMENT_3D('',#36053,#22904,#22905);
#19067=AXIS2_PLACEMENT_3D('',#36054,#22906,#22907);
#19068=AXIS2_PLACEMENT_3D('',#36056,#22909,#22910);
#19069=AXIS2_PLACEMENT_3D('',#36057,#22911,#22912);
#19070=AXIS2_PLACEMENT_3D('',#36059,#22914,#22915);
#19071=AXIS2_PLACEMENT_3D('',#36060,#22916,#22917);
#19072=AXIS2_PLACEMENT_3D('',#36062,#22919,#22920);
#19073=AXIS2_PLACEMENT_3D('',#36063,#22921,#22922);
#19074=AXIS2_PLACEMENT_3D('',#36065,#22924,#22925);
#19075=AXIS2_PLACEMENT_3D('',#36066,#22926,#22927);
#19076=AXIS2_PLACEMENT_3D('',#36068,#22929,#22930);
#19077=AXIS2_PLACEMENT_3D('',#36069,#22931,#22932);
#19078=AXIS2_PLACEMENT_3D('',#36071,#22934,#22935);
#19079=AXIS2_PLACEMENT_3D('',#36072,#22936,#22937);
#19080=AXIS2_PLACEMENT_3D('',#36074,#22939,#22940);
#19081=AXIS2_PLACEMENT_3D('',#36075,#22941,#22942);
#19082=AXIS2_PLACEMENT_3D('',#36077,#22944,#22945);
#19083=AXIS2_PLACEMENT_3D('',#36078,#22946,#22947);
#19084=AXIS2_PLACEMENT_3D('',#36080,#22949,#22950);
#19085=AXIS2_PLACEMENT_3D('',#36081,#22951,#22952);
#19086=AXIS2_PLACEMENT_3D('',#36083,#22954,#22955);
#19087=AXIS2_PLACEMENT_3D('',#36084,#22956,#22957);
#19088=AXIS2_PLACEMENT_3D('',#36086,#22959,#22960);
#19089=AXIS2_PLACEMENT_3D('',#36087,#22961,#22962);
#19090=AXIS2_PLACEMENT_3D('',#36089,#22964,#22965);
#19091=AXIS2_PLACEMENT_3D('',#36090,#22966,#22967);
#19092=AXIS2_PLACEMENT_3D('',#36092,#22969,#22970);
#19093=AXIS2_PLACEMENT_3D('',#36093,#22971,#22972);
#19094=AXIS2_PLACEMENT_3D('',#36095,#22974,#22975);
#19095=AXIS2_PLACEMENT_3D('',#36096,#22976,#22977);
#19096=AXIS2_PLACEMENT_3D('',#36098,#22979,#22980);
#19097=AXIS2_PLACEMENT_3D('',#36099,#22981,#22982);
#19098=AXIS2_PLACEMENT_3D('',#36101,#22984,#22985);
#19099=AXIS2_PLACEMENT_3D('',#36102,#22986,#22987);
#19100=AXIS2_PLACEMENT_3D('',#36104,#22989,#22990);
#19101=AXIS2_PLACEMENT_3D('',#36105,#22991,#22992);
#19102=AXIS2_PLACEMENT_3D('',#36107,#22994,#22995);
#19103=AXIS2_PLACEMENT_3D('',#36108,#22996,#22997);
#19104=AXIS2_PLACEMENT_3D('',#36110,#22999,#23000);
#19105=AXIS2_PLACEMENT_3D('',#36111,#23001,#23002);
#19106=AXIS2_PLACEMENT_3D('',#36113,#23004,#23005);
#19107=AXIS2_PLACEMENT_3D('',#36114,#23006,#23007);
#19108=AXIS2_PLACEMENT_3D('',#36116,#23009,#23010);
#19109=AXIS2_PLACEMENT_3D('',#36117,#23011,#23012);
#19110=AXIS2_PLACEMENT_3D('',#36119,#23014,#23015);
#19111=AXIS2_PLACEMENT_3D('',#36120,#23016,#23017);
#19112=AXIS2_PLACEMENT_3D('',#36122,#23019,#23020);
#19113=AXIS2_PLACEMENT_3D('',#36123,#23021,#23022);
#19114=AXIS2_PLACEMENT_3D('',#36125,#23024,#23025);
#19115=AXIS2_PLACEMENT_3D('',#36126,#23026,#23027);
#19116=AXIS2_PLACEMENT_3D('',#36128,#23029,#23030);
#19117=AXIS2_PLACEMENT_3D('',#36129,#23031,#23032);
#19118=AXIS2_PLACEMENT_3D('',#36131,#23034,#23035);
#19119=AXIS2_PLACEMENT_3D('',#36132,#23036,#23037);
#19120=AXIS2_PLACEMENT_3D('',#36134,#23039,#23040);
#19121=AXIS2_PLACEMENT_3D('',#36135,#23041,#23042);
#19122=AXIS2_PLACEMENT_3D('',#36137,#23044,#23045);
#19123=AXIS2_PLACEMENT_3D('',#36138,#23046,#23047);
#19124=AXIS2_PLACEMENT_3D('',#36140,#23049,#23050);
#19125=AXIS2_PLACEMENT_3D('',#36141,#23051,#23052);
#19126=AXIS2_PLACEMENT_3D('',#36143,#23054,#23055);
#19127=AXIS2_PLACEMENT_3D('',#36144,#23056,#23057);
#19128=AXIS2_PLACEMENT_3D('',#36146,#23059,#23060);
#19129=AXIS2_PLACEMENT_3D('',#36147,#23061,#23062);
#19130=AXIS2_PLACEMENT_3D('',#36149,#23064,#23065);
#19131=AXIS2_PLACEMENT_3D('',#36150,#23066,#23067);
#19132=AXIS2_PLACEMENT_3D('',#36152,#23069,#23070);
#19133=AXIS2_PLACEMENT_3D('',#36153,#23071,#23072);
#19134=AXIS2_PLACEMENT_3D('',#36155,#23074,#23075);
#19135=AXIS2_PLACEMENT_3D('',#36156,#23076,#23077);
#19136=AXIS2_PLACEMENT_3D('',#36158,#23079,#23080);
#19137=AXIS2_PLACEMENT_3D('',#36159,#23081,#23082);
#19138=AXIS2_PLACEMENT_3D('',#36161,#23084,#23085);
#19139=AXIS2_PLACEMENT_3D('',#36162,#23086,#23087);
#19140=AXIS2_PLACEMENT_3D('',#36164,#23089,#23090);
#19141=AXIS2_PLACEMENT_3D('',#36165,#23091,#23092);
#19142=AXIS2_PLACEMENT_3D('',#36167,#23094,#23095);
#19143=AXIS2_PLACEMENT_3D('',#36168,#23096,#23097);
#19144=AXIS2_PLACEMENT_3D('',#36170,#23099,#23100);
#19145=AXIS2_PLACEMENT_3D('',#36171,#23101,#23102);
#19146=AXIS2_PLACEMENT_3D('',#36173,#23104,#23105);
#19147=AXIS2_PLACEMENT_3D('',#36174,#23106,#23107);
#19148=AXIS2_PLACEMENT_3D('',#36176,#23109,#23110);
#19149=AXIS2_PLACEMENT_3D('',#36177,#23111,#23112);
#19150=AXIS2_PLACEMENT_3D('',#36179,#23114,#23115);
#19151=AXIS2_PLACEMENT_3D('',#36180,#23116,#23117);
#19152=AXIS2_PLACEMENT_3D('',#36182,#23119,#23120);
#19153=AXIS2_PLACEMENT_3D('',#36183,#23121,#23122);
#19154=AXIS2_PLACEMENT_3D('',#36185,#23124,#23125);
#19155=AXIS2_PLACEMENT_3D('',#36186,#23126,#23127);
#19156=AXIS2_PLACEMENT_3D('',#36188,#23129,#23130);
#19157=AXIS2_PLACEMENT_3D('',#36189,#23131,#23132);
#19158=AXIS2_PLACEMENT_3D('',#36191,#23134,#23135);
#19159=AXIS2_PLACEMENT_3D('',#36192,#23136,#23137);
#19160=AXIS2_PLACEMENT_3D('',#36194,#23139,#23140);
#19161=AXIS2_PLACEMENT_3D('',#36195,#23141,#23142);
#19162=AXIS2_PLACEMENT_3D('',#36197,#23144,#23145);
#19163=AXIS2_PLACEMENT_3D('',#36198,#23146,#23147);
#19164=AXIS2_PLACEMENT_3D('',#36200,#23149,#23150);
#19165=AXIS2_PLACEMENT_3D('',#36201,#23151,#23152);
#19166=AXIS2_PLACEMENT_3D('',#36203,#23154,#23155);
#19167=AXIS2_PLACEMENT_3D('',#36204,#23156,#23157);
#19168=AXIS2_PLACEMENT_3D('',#36206,#23159,#23160);
#19169=AXIS2_PLACEMENT_3D('',#36207,#23161,#23162);
#19170=AXIS2_PLACEMENT_3D('',#36209,#23164,#23165);
#19171=AXIS2_PLACEMENT_3D('',#36210,#23166,#23167);
#19172=AXIS2_PLACEMENT_3D('',#36212,#23169,#23170);
#19173=AXIS2_PLACEMENT_3D('',#36213,#23171,#23172);
#19174=AXIS2_PLACEMENT_3D('',#36215,#23174,#23175);
#19175=AXIS2_PLACEMENT_3D('',#36216,#23176,#23177);
#19176=AXIS2_PLACEMENT_3D('',#36218,#23179,#23180);
#19177=AXIS2_PLACEMENT_3D('',#36219,#23181,#23182);
#19178=AXIS2_PLACEMENT_3D('',#36221,#23184,#23185);
#19179=AXIS2_PLACEMENT_3D('',#36222,#23186,#23187);
#19180=AXIS2_PLACEMENT_3D('',#36224,#23189,#23190);
#19181=AXIS2_PLACEMENT_3D('',#36225,#23191,#23192);
#19182=AXIS2_PLACEMENT_3D('',#36227,#23194,#23195);
#19183=AXIS2_PLACEMENT_3D('',#36228,#23196,#23197);
#19184=AXIS2_PLACEMENT_3D('',#36230,#23199,#23200);
#19185=AXIS2_PLACEMENT_3D('',#36231,#23201,#23202);
#19186=AXIS2_PLACEMENT_3D('',#36233,#23204,#23205);
#19187=AXIS2_PLACEMENT_3D('',#36234,#23206,#23207);
#19188=AXIS2_PLACEMENT_3D('',#36236,#23209,#23210);
#19189=AXIS2_PLACEMENT_3D('',#36237,#23211,#23212);
#19190=AXIS2_PLACEMENT_3D('',#36240,#23213,#23214);
#19191=AXIS2_PLACEMENT_3D('',#36253,#23215,#23216);
#19192=AXIS2_PLACEMENT_3D('',#36266,#23217,#23218);
#19193=AXIS2_PLACEMENT_3D('',#36268,#23219,#23220);
#19194=AXIS2_PLACEMENT_3D('',#36270,#23221,#23222);
#19195=AXIS2_PLACEMENT_3D('',#36271,#23223,#23224);
#19196=AXIS2_PLACEMENT_3D('',#36273,#23225,#23226);
#19197=AXIS2_PLACEMENT_3D('',#36286,#23227,#23228);
#19198=AXIS2_PLACEMENT_3D('',#36297,#23229,#23230);
#19199=AXIS2_PLACEMENT_3D('',#36299,#23231,#23232);
#19200=AXIS2_PLACEMENT_3D('',#36301,#23234,#23235);
#19201=AXIS2_PLACEMENT_3D('',#36303,#23236,#23237);
#19202=AXIS2_PLACEMENT_3D('',#36306,#23239,#23240);
#19203=AXIS2_PLACEMENT_3D('',#36307,#23241,#23242);
#19204=AXIS2_PLACEMENT_3D('',#36309,#23244,#23245);
#19205=AXIS2_PLACEMENT_3D('',#36310,#23246,#23247);
#19206=AXIS2_PLACEMENT_3D('',#36312,#23249,#23250);
#19207=AXIS2_PLACEMENT_3D('',#36313,#23251,#23252);
#19208=AXIS2_PLACEMENT_3D('',#36315,#23254,#23255);
#19209=AXIS2_PLACEMENT_3D('',#36317,#23257,#23258);
#19210=AXIS2_PLACEMENT_3D('',#36318,#23259,#23260);
#19211=AXIS2_PLACEMENT_3D('',#36320,#23261,#23262);
#19212=AXIS2_PLACEMENT_3D('',#36322,#23263,#23264);
#19213=AXIS2_PLACEMENT_3D('',#36323,#23265,#23266);
#19214=AXIS2_PLACEMENT_3D('',#36324,#23267,#23268);
#19215=AXIS2_PLACEMENT_3D('',#36327,#23269,#23270);
#19216=AXIS2_PLACEMENT_3D('',#36328,#23271,#23272);
#19217=AXIS2_PLACEMENT_3D('',#36331,#23274,#23275);
#19218=AXIS2_PLACEMENT_3D('',#36332,#23276,#23277);
#19219=AXIS2_PLACEMENT_3D('',#36335,#23278,#23279);
#19220=AXIS2_PLACEMENT_3D('',#36336,#23280,#23281);
#19221=AXIS2_PLACEMENT_3D('',#36340,#23283,#23284);
#19222=AXIS2_PLACEMENT_3D('',#36341,#23285,#23286);
#19223=AXIS2_PLACEMENT_3D('',#36342,#23287,#23288);
#19224=AXIS2_PLACEMENT_3D('',#36344,#23290,#23291);
#19225=AXIS2_PLACEMENT_3D('',#36347,#23292,#23293);
#19226=AXIS2_PLACEMENT_3D('',#36348,#23294,#23295);
#19227=AXIS2_PLACEMENT_3D('',#36350,#23297,#23298);
#19228=AXIS2_PLACEMENT_3D('',#36353,#23299,#23300);
#19229=AXIS2_PLACEMENT_3D('',#36354,#23301,#23302);
#19230=AXIS2_PLACEMENT_3D('',#36358,#23304,#23305);
#19231=AXIS2_PLACEMENT_3D('',#36359,#23306,#23307);
#19232=AXIS2_PLACEMENT_3D('',#36360,#23308,#23309);
#19233=AXIS2_PLACEMENT_3D('',#36362,#23311,#23312);
#19234=AXIS2_PLACEMENT_3D('',#36365,#23313,#23314);
#19235=AXIS2_PLACEMENT_3D('',#36366,#23315,#23316);
#19236=AXIS2_PLACEMENT_3D('',#36368,#23318,#23319);
#19237=AXIS2_PLACEMENT_3D('',#36371,#23320,#23321);
#19238=AXIS2_PLACEMENT_3D('',#36372,#23322,#23323);
#19239=AXIS2_PLACEMENT_3D('',#36376,#23325,#23326);
#19240=AXIS2_PLACEMENT_3D('',#36377,#23327,#23328);
#19241=AXIS2_PLACEMENT_3D('',#36378,#23329,#23330);
#19242=AXIS2_PLACEMENT_3D('',#36380,#23332,#23333);
#19243=AXIS2_PLACEMENT_3D('',#36383,#23334,#23335);
#19244=AXIS2_PLACEMENT_3D('',#36384,#23336,#23337);
#19245=AXIS2_PLACEMENT_3D('',#36386,#23339,#23340);
#19246=AXIS2_PLACEMENT_3D('',#36389,#23341,#23342);
#19247=AXIS2_PLACEMENT_3D('',#36390,#23343,#23344);
#19248=AXIS2_PLACEMENT_3D('',#36394,#23346,#23347);
#19249=AXIS2_PLACEMENT_3D('',#36395,#23348,#23349);
#19250=AXIS2_PLACEMENT_3D('',#36396,#23350,#23351);
#19251=AXIS2_PLACEMENT_3D('',#36398,#23353,#23354);
#19252=AXIS2_PLACEMENT_3D('',#36401,#23355,#23356);
#19253=AXIS2_PLACEMENT_3D('',#36402,#23357,#23358);
#19254=AXIS2_PLACEMENT_3D('',#36404,#23360,#23361);
#19255=AXIS2_PLACEMENT_3D('',#36407,#23362,#23363);
#19256=AXIS2_PLACEMENT_3D('',#36408,#23364,#23365);
#19257=AXIS2_PLACEMENT_3D('',#36412,#23367,#23368);
#19258=AXIS2_PLACEMENT_3D('',#36413,#23369,#23370);
#19259=AXIS2_PLACEMENT_3D('',#36414,#23371,#23372);
#19260=AXIS2_PLACEMENT_3D('',#36416,#23374,#23375);
#19261=AXIS2_PLACEMENT_3D('',#36419,#23376,#23377);
#19262=AXIS2_PLACEMENT_3D('',#36420,#23378,#23379);
#19263=AXIS2_PLACEMENT_3D('',#36422,#23381,#23382);
#19264=AXIS2_PLACEMENT_3D('',#36425,#23383,#23384);
#19265=AXIS2_PLACEMENT_3D('',#36426,#23385,#23386);
#19266=AXIS2_PLACEMENT_3D('',#36430,#23388,#23389);
#19267=AXIS2_PLACEMENT_3D('',#36431,#23390,#23391);
#19268=AXIS2_PLACEMENT_3D('',#36432,#23392,#23393);
#19269=AXIS2_PLACEMENT_3D('',#36434,#23395,#23396);
#19270=AXIS2_PLACEMENT_3D('',#36437,#23397,#23398);
#19271=AXIS2_PLACEMENT_3D('',#36438,#23399,#23400);
#19272=AXIS2_PLACEMENT_3D('',#36440,#23402,#23403);
#19273=AXIS2_PLACEMENT_3D('',#36443,#23404,#23405);
#19274=AXIS2_PLACEMENT_3D('',#36444,#23406,#23407);
#19275=AXIS2_PLACEMENT_3D('',#36448,#23409,#23410);
#19276=AXIS2_PLACEMENT_3D('',#36449,#23411,#23412);
#19277=AXIS2_PLACEMENT_3D('',#36450,#23413,#23414);
#19278=AXIS2_PLACEMENT_3D('',#36452,#23416,#23417);
#19279=AXIS2_PLACEMENT_3D('',#36455,#23418,#23419);
#19280=AXIS2_PLACEMENT_3D('',#36456,#23420,#23421);
#19281=AXIS2_PLACEMENT_3D('',#36458,#23423,#23424);
#19282=AXIS2_PLACEMENT_3D('',#36461,#23425,#23426);
#19283=AXIS2_PLACEMENT_3D('',#36462,#23427,#23428);
#19284=AXIS2_PLACEMENT_3D('',#36466,#23430,#23431);
#19285=AXIS2_PLACEMENT_3D('',#36467,#23432,#23433);
#19286=AXIS2_PLACEMENT_3D('',#36468,#23434,#23435);
#19287=AXIS2_PLACEMENT_3D('',#36470,#23437,#23438);
#19288=AXIS2_PLACEMENT_3D('',#36473,#23439,#23440);
#19289=AXIS2_PLACEMENT_3D('',#36474,#23441,#23442);
#19290=AXIS2_PLACEMENT_3D('',#36476,#23444,#23445);
#19291=AXIS2_PLACEMENT_3D('',#36479,#23446,#23447);
#19292=AXIS2_PLACEMENT_3D('',#36480,#23448,#23449);
#19293=AXIS2_PLACEMENT_3D('',#36484,#23451,#23452);
#19294=AXIS2_PLACEMENT_3D('',#36485,#23453,#23454);
#19295=AXIS2_PLACEMENT_3D('',#36486,#23455,#23456);
#19296=AXIS2_PLACEMENT_3D('',#36488,#23458,#23459);
#19297=AXIS2_PLACEMENT_3D('',#36491,#23460,#23461);
#19298=AXIS2_PLACEMENT_3D('',#36492,#23462,#23463);
#19299=AXIS2_PLACEMENT_3D('',#36494,#23465,#23466);
#19300=AXIS2_PLACEMENT_3D('',#36497,#23467,#23468);
#19301=AXIS2_PLACEMENT_3D('',#36498,#23469,#23470);
#19302=AXIS2_PLACEMENT_3D('',#36502,#23472,#23473);
#19303=AXIS2_PLACEMENT_3D('',#36503,#23474,#23475);
#19304=AXIS2_PLACEMENT_3D('',#36504,#23476,#23477);
#19305=AXIS2_PLACEMENT_3D('',#36506,#23479,#23480);
#19306=AXIS2_PLACEMENT_3D('',#36509,#23481,#23482);
#19307=AXIS2_PLACEMENT_3D('',#36510,#23483,#23484);
#19308=AXIS2_PLACEMENT_3D('',#36512,#23486,#23487);
#19309=AXIS2_PLACEMENT_3D('',#36515,#23488,#23489);
#19310=AXIS2_PLACEMENT_3D('',#36516,#23490,#23491);
#19311=AXIS2_PLACEMENT_3D('',#36520,#23493,#23494);
#19312=AXIS2_PLACEMENT_3D('',#36521,#23495,#23496);
#19313=AXIS2_PLACEMENT_3D('',#36522,#23497,#23498);
#19314=AXIS2_PLACEMENT_3D('',#36524,#23500,#23501);
#19315=AXIS2_PLACEMENT_3D('',#36527,#23502,#23503);
#19316=AXIS2_PLACEMENT_3D('',#36528,#23504,#23505);
#19317=AXIS2_PLACEMENT_3D('',#36530,#23507,#23508);
#19318=AXIS2_PLACEMENT_3D('',#36533,#23509,#23510);
#19319=AXIS2_PLACEMENT_3D('',#36534,#23511,#23512);
#19320=AXIS2_PLACEMENT_3D('',#36538,#23514,#23515);
#19321=AXIS2_PLACEMENT_3D('',#36539,#23516,#23517);
#19322=AXIS2_PLACEMENT_3D('',#36540,#23518,#23519);
#19323=AXIS2_PLACEMENT_3D('',#36542,#23521,#23522);
#19324=AXIS2_PLACEMENT_3D('',#36545,#23523,#23524);
#19325=AXIS2_PLACEMENT_3D('',#36546,#23525,#23526);
#19326=AXIS2_PLACEMENT_3D('',#36548,#23528,#23529);
#19327=AXIS2_PLACEMENT_3D('',#36551,#23530,#23531);
#19328=AXIS2_PLACEMENT_3D('',#36552,#23532,#23533);
#19329=AXIS2_PLACEMENT_3D('',#36556,#23535,#23536);
#19330=AXIS2_PLACEMENT_3D('',#36557,#23537,#23538);
#19331=AXIS2_PLACEMENT_3D('',#36558,#23539,#23540);
#19332=AXIS2_PLACEMENT_3D('',#36560,#23542,#23543);
#19333=AXIS2_PLACEMENT_3D('',#36563,#23545,#23546);
#19334=AXIS2_PLACEMENT_3D('',#36564,#23547,#23548);
#19335=AXIS2_PLACEMENT_3D('',#36571,#23549,#23550);
#19336=AXIS2_PLACEMENT_3D('',#36581,#23551,#23552);
#19337=AXIS2_PLACEMENT_3D('',#36591,#23553,#23554);
#19338=AXIS2_PLACEMENT_3D('',#36601,#23555,#23556);
#19339=AXIS2_PLACEMENT_3D('',#36611,#23557,#23558);
#19340=AXIS2_PLACEMENT_3D('',#36621,#23559,#23560);
#19341=AXIS2_PLACEMENT_3D('',#36631,#23561,#23562);
#19342=AXIS2_PLACEMENT_3D('',#36641,#23563,#23564);
#19343=AXIS2_PLACEMENT_3D('',#36651,#23565,#23566);
#19344=AXIS2_PLACEMENT_3D('',#36661,#23567,#23568);
#19345=AXIS2_PLACEMENT_3D('',#36671,#23569,#23570);
#19346=AXIS2_PLACEMENT_3D('',#36681,#23571,#23572);
#19347=AXIS2_PLACEMENT_3D('',#36691,#23573,#23574);
#19348=AXIS2_PLACEMENT_3D('',#36701,#23575,#23576);
#19349=AXIS2_PLACEMENT_3D('',#36711,#23577,#23578);
#19350=AXIS2_PLACEMENT_3D('',#36721,#23579,#23580);
#19351=AXIS2_PLACEMENT_3D('',#36731,#23581,#23582);
#19352=AXIS2_PLACEMENT_3D('',#36741,#23583,#23584);
#19353=AXIS2_PLACEMENT_3D('',#36751,#23585,#23586);
#19354=AXIS2_PLACEMENT_3D('',#36761,#23587,#23588);
#19355=AXIS2_PLACEMENT_3D('',#36771,#23589,#23590);
#19356=AXIS2_PLACEMENT_3D('',#36781,#23591,#23592);
#19357=AXIS2_PLACEMENT_3D('',#36791,#23593,#23594);
#19358=AXIS2_PLACEMENT_3D('',#36801,#23595,#23596);
#19359=AXIS2_PLACEMENT_3D('',#36811,#23597,#23598);
#19360=AXIS2_PLACEMENT_3D('',#36821,#23599,#23600);
#19361=AXIS2_PLACEMENT_3D('',#36831,#23601,#23602);
#19362=AXIS2_PLACEMENT_3D('',#36841,#23603,#23604);
#19363=AXIS2_PLACEMENT_3D('',#36851,#23605,#23606);
#19364=AXIS2_PLACEMENT_3D('',#36861,#23607,#23608);
#19365=AXIS2_PLACEMENT_3D('',#36871,#23609,#23610);
#19366=AXIS2_PLACEMENT_3D('',#36881,#23611,#23612);
#19367=AXIS2_PLACEMENT_3D('',#36891,#23613,#23614);
#19368=AXIS2_PLACEMENT_3D('',#36901,#23615,#23616);
#19369=AXIS2_PLACEMENT_3D('',#36911,#23617,#23618);
#19370=AXIS2_PLACEMENT_3D('',#36921,#23619,#23620);
#19371=AXIS2_PLACEMENT_3D('',#36931,#23621,#23622);
#19372=AXIS2_PLACEMENT_3D('',#36941,#23623,#23624);
#19373=AXIS2_PLACEMENT_3D('',#36951,#23625,#23626);
#19374=AXIS2_PLACEMENT_3D('',#36958,#23628,#23629);
#19375=AXIS2_PLACEMENT_3D('',#36968,#23630,#23631);
#19376=AXIS2_PLACEMENT_3D('',#36978,#23632,#23633);
#19377=AXIS2_PLACEMENT_3D('',#36988,#23634,#23635);
#19378=AXIS2_PLACEMENT_3D('',#36998,#23636,#23637);
#19379=AXIS2_PLACEMENT_3D('',#37008,#23638,#23639);
#19380=AXIS2_PLACEMENT_3D('',#37018,#23640,#23641);
#19381=AXIS2_PLACEMENT_3D('',#37028,#23642,#23643);
#19382=AXIS2_PLACEMENT_3D('',#37038,#23644,#23645);
#19383=AXIS2_PLACEMENT_3D('',#37048,#23646,#23647);
#19384=AXIS2_PLACEMENT_3D('',#37058,#23648,#23649);
#19385=AXIS2_PLACEMENT_3D('',#37068,#23650,#23651);
#19386=AXIS2_PLACEMENT_3D('',#37078,#23652,#23653);
#19387=AXIS2_PLACEMENT_3D('',#37088,#23654,#23655);
#19388=AXIS2_PLACEMENT_3D('',#37098,#23656,#23657);
#19389=AXIS2_PLACEMENT_3D('',#37108,#23658,#23659);
#19390=AXIS2_PLACEMENT_3D('',#37118,#23660,#23661);
#19391=AXIS2_PLACEMENT_3D('',#37128,#23662,#23663);
#19392=AXIS2_PLACEMENT_3D('',#37138,#23664,#23665);
#19393=AXIS2_PLACEMENT_3D('',#37148,#23666,#23667);
#19394=AXIS2_PLACEMENT_3D('',#37158,#23668,#23669);
#19395=AXIS2_PLACEMENT_3D('',#37168,#23670,#23671);
#19396=AXIS2_PLACEMENT_3D('',#37178,#23672,#23673);
#19397=AXIS2_PLACEMENT_3D('',#37188,#23674,#23675);
#19398=AXIS2_PLACEMENT_3D('',#37198,#23676,#23677);
#19399=AXIS2_PLACEMENT_3D('',#37208,#23678,#23679);
#19400=AXIS2_PLACEMENT_3D('',#37218,#23680,#23681);
#19401=AXIS2_PLACEMENT_3D('',#37228,#23682,#23683);
#19402=AXIS2_PLACEMENT_3D('',#37238,#23684,#23685);
#19403=AXIS2_PLACEMENT_3D('',#37248,#23686,#23687);
#19404=AXIS2_PLACEMENT_3D('',#37258,#23688,#23689);
#19405=AXIS2_PLACEMENT_3D('',#37268,#23690,#23691);
#19406=AXIS2_PLACEMENT_3D('',#37278,#23692,#23693);
#19407=AXIS2_PLACEMENT_3D('',#37288,#23694,#23695);
#19408=AXIS2_PLACEMENT_3D('',#37298,#23696,#23697);
#19409=AXIS2_PLACEMENT_3D('',#37308,#23698,#23699);
#19410=AXIS2_PLACEMENT_3D('',#37318,#23700,#23701);
#19411=AXIS2_PLACEMENT_3D('',#37328,#23702,#23703);
#19412=AXIS2_PLACEMENT_3D('',#37338,#23704,#23705);
#19413=AXIS2_PLACEMENT_3D('',#37342,#23706,#23707);
#19414=AXIS2_PLACEMENT_3D('',#37349,#23708,#23709);
#19415=AXIS2_PLACEMENT_3D('',#37359,#23710,#23711);
#19416=AXIS2_PLACEMENT_3D('',#37369,#23712,#23713);
#19417=AXIS2_PLACEMENT_3D('',#37379,#23714,#23715);
#19418=AXIS2_PLACEMENT_3D('',#37389,#23716,#23717);
#19419=AXIS2_PLACEMENT_3D('',#37399,#23718,#23719);
#19420=AXIS2_PLACEMENT_3D('',#37409,#23720,#23721);
#19421=AXIS2_PLACEMENT_3D('',#37419,#23722,#23723);
#19422=AXIS2_PLACEMENT_3D('',#37429,#23724,#23725);
#19423=AXIS2_PLACEMENT_3D('',#37439,#23726,#23727);
#19424=AXIS2_PLACEMENT_3D('',#37449,#23728,#23729);
#19425=AXIS2_PLACEMENT_3D('',#37459,#23730,#23731);
#19426=AXIS2_PLACEMENT_3D('',#37469,#23732,#23733);
#19427=AXIS2_PLACEMENT_3D('',#37479,#23734,#23735);
#19428=AXIS2_PLACEMENT_3D('',#37489,#23736,#23737);
#19429=AXIS2_PLACEMENT_3D('',#37499,#23738,#23739);
#19430=AXIS2_PLACEMENT_3D('',#37509,#23740,#23741);
#19431=AXIS2_PLACEMENT_3D('',#37519,#23742,#23743);
#19432=AXIS2_PLACEMENT_3D('',#37529,#23744,#23745);
#19433=AXIS2_PLACEMENT_3D('',#37539,#23746,#23747);
#19434=AXIS2_PLACEMENT_3D('',#37549,#23748,#23749);
#19435=AXIS2_PLACEMENT_3D('',#37559,#23750,#23751);
#19436=AXIS2_PLACEMENT_3D('',#37569,#23752,#23753);
#19437=AXIS2_PLACEMENT_3D('',#37579,#23754,#23755);
#19438=AXIS2_PLACEMENT_3D('',#37589,#23756,#23757);
#19439=AXIS2_PLACEMENT_3D('',#37599,#23758,#23759);
#19440=AXIS2_PLACEMENT_3D('',#37609,#23760,#23761);
#19441=AXIS2_PLACEMENT_3D('',#37619,#23762,#23763);
#19442=AXIS2_PLACEMENT_3D('',#37629,#23764,#23765);
#19443=AXIS2_PLACEMENT_3D('',#37639,#23766,#23767);
#19444=AXIS2_PLACEMENT_3D('',#37649,#23768,#23769);
#19445=AXIS2_PLACEMENT_3D('',#37659,#23770,#23771);
#19446=AXIS2_PLACEMENT_3D('',#37669,#23772,#23773);
#19447=AXIS2_PLACEMENT_3D('',#37679,#23774,#23775);
#19448=AXIS2_PLACEMENT_3D('',#37689,#23776,#23777);
#19449=AXIS2_PLACEMENT_3D('',#37699,#23778,#23779);
#19450=AXIS2_PLACEMENT_3D('',#37709,#23780,#23781);
#19451=AXIS2_PLACEMENT_3D('',#37719,#23782,#23783);
#19452=AXIS2_PLACEMENT_3D('',#37729,#23784,#23785);
#19453=AXIS2_PLACEMENT_3D('',#37736,#23787,#23788);
#19454=AXIS2_PLACEMENT_3D('',#37746,#23789,#23790);
#19455=AXIS2_PLACEMENT_3D('',#37756,#23791,#23792);
#19456=AXIS2_PLACEMENT_3D('',#37766,#23793,#23794);
#19457=AXIS2_PLACEMENT_3D('',#37776,#23795,#23796);
#19458=AXIS2_PLACEMENT_3D('',#37786,#23797,#23798);
#19459=AXIS2_PLACEMENT_3D('',#37796,#23799,#23800);
#19460=AXIS2_PLACEMENT_3D('',#37806,#23801,#23802);
#19461=AXIS2_PLACEMENT_3D('',#37816,#23803,#23804);
#19462=AXIS2_PLACEMENT_3D('',#37826,#23805,#23806);
#19463=AXIS2_PLACEMENT_3D('',#37836,#23807,#23808);
#19464=AXIS2_PLACEMENT_3D('',#37846,#23809,#23810);
#19465=AXIS2_PLACEMENT_3D('',#37856,#23811,#23812);
#19466=AXIS2_PLACEMENT_3D('',#37866,#23813,#23814);
#19467=AXIS2_PLACEMENT_3D('',#37876,#23815,#23816);
#19468=AXIS2_PLACEMENT_3D('',#37886,#23817,#23818);
#19469=AXIS2_PLACEMENT_3D('',#37896,#23819,#23820);
#19470=AXIS2_PLACEMENT_3D('',#37906,#23821,#23822);
#19471=AXIS2_PLACEMENT_3D('',#37916,#23823,#23824);
#19472=AXIS2_PLACEMENT_3D('',#37926,#23825,#23826);
#19473=AXIS2_PLACEMENT_3D('',#37936,#23827,#23828);
#19474=AXIS2_PLACEMENT_3D('',#37946,#23829,#23830);
#19475=AXIS2_PLACEMENT_3D('',#37956,#23831,#23832);
#19476=AXIS2_PLACEMENT_3D('',#37966,#23833,#23834);
#19477=AXIS2_PLACEMENT_3D('',#37976,#23835,#23836);
#19478=AXIS2_PLACEMENT_3D('',#37986,#23837,#23838);
#19479=AXIS2_PLACEMENT_3D('',#37996,#23839,#23840);
#19480=AXIS2_PLACEMENT_3D('',#38006,#23841,#23842);
#19481=AXIS2_PLACEMENT_3D('',#38016,#23843,#23844);
#19482=AXIS2_PLACEMENT_3D('',#38026,#23845,#23846);
#19483=AXIS2_PLACEMENT_3D('',#38036,#23847,#23848);
#19484=AXIS2_PLACEMENT_3D('',#38046,#23849,#23850);
#19485=AXIS2_PLACEMENT_3D('',#38056,#23851,#23852);
#19486=AXIS2_PLACEMENT_3D('',#38066,#23853,#23854);
#19487=AXIS2_PLACEMENT_3D('',#38076,#23855,#23856);
#19488=AXIS2_PLACEMENT_3D('',#38086,#23857,#23858);
#19489=AXIS2_PLACEMENT_3D('',#38096,#23859,#23860);
#19490=AXIS2_PLACEMENT_3D('',#38106,#23861,#23862);
#19491=AXIS2_PLACEMENT_3D('',#38116,#23863,#23864);
#19492=AXIS2_PLACEMENT_3D('',#38120,#23865,#23866);
#19493=AXIS2_PLACEMENT_3D('',#38122,#23867,#23868);
#19494=AXIS2_PLACEMENT_3D('',#38124,#23870,#23871);
#19495=AXIS2_PLACEMENT_3D('',#38127,#23874,#23875);
#19496=AXIS2_PLACEMENT_3D('',#38130,#23878,#23879);
#19497=AXIS2_PLACEMENT_3D('',#38133,#23882,#23883);
#19498=AXIS2_PLACEMENT_3D('',#38136,#23886,#23887);
#19499=AXIS2_PLACEMENT_3D('',#38139,#23890,#23891);
#19500=AXIS2_PLACEMENT_3D('',#38142,#23894,#23895);
#19501=AXIS2_PLACEMENT_3D('',#38145,#23898,#23899);
#19502=AXIS2_PLACEMENT_3D('',#38148,#23902,#23903);
#19503=AXIS2_PLACEMENT_3D('',#38151,#23906,#23907);
#19504=AXIS2_PLACEMENT_3D('',#38154,#23910,#23911);
#19505=AXIS2_PLACEMENT_3D('',#38157,#23914,#23915);
#19506=AXIS2_PLACEMENT_3D('',#38160,#23918,#23919);
#19507=AXIS2_PLACEMENT_3D('',#38163,#23922,#23923);
#19508=AXIS2_PLACEMENT_3D('',#38166,#23926,#23927);
#19509=AXIS2_PLACEMENT_3D('',#38169,#23930,#23931);
#19510=AXIS2_PLACEMENT_3D('',#38172,#23934,#23935);
#19511=AXIS2_PLACEMENT_3D('',#38175,#23938,#23939);
#19512=AXIS2_PLACEMENT_3D('',#38178,#23942,#23943);
#19513=AXIS2_PLACEMENT_3D('',#38181,#23946,#23947);
#19514=AXIS2_PLACEMENT_3D('',#38184,#23950,#23951);
#19515=AXIS2_PLACEMENT_3D('',#38187,#23954,#23955);
#19516=AXIS2_PLACEMENT_3D('',#38190,#23958,#23959);
#19517=AXIS2_PLACEMENT_3D('',#38193,#23962,#23963);
#19518=AXIS2_PLACEMENT_3D('',#38196,#23966,#23967);
#19519=AXIS2_PLACEMENT_3D('',#38199,#23970,#23971);
#19520=AXIS2_PLACEMENT_3D('',#38202,#23974,#23975);
#19521=AXIS2_PLACEMENT_3D('',#38205,#23978,#23979);
#19522=AXIS2_PLACEMENT_3D('',#38208,#23982,#23983);
#19523=AXIS2_PLACEMENT_3D('',#38211,#23986,#23987);
#19524=AXIS2_PLACEMENT_3D('',#38214,#23990,#23991);
#19525=AXIS2_PLACEMENT_3D('',#38217,#23994,#23995);
#19526=AXIS2_PLACEMENT_3D('',#38220,#23998,#23999);
#19527=AXIS2_PLACEMENT_3D('',#38223,#24002,#24003);
#19528=AXIS2_PLACEMENT_3D('',#38226,#24006,#24007);
#19529=AXIS2_PLACEMENT_3D('',#38229,#24010,#24011);
#19530=AXIS2_PLACEMENT_3D('',#38232,#24014,#24015);
#19531=AXIS2_PLACEMENT_3D('',#38235,#24018,#24019);
#19532=AXIS2_PLACEMENT_3D('',#38238,#24022,#24023);
#19533=AXIS2_PLACEMENT_3D('',#38241,#24026,#24027);
#19534=AXIS2_PLACEMENT_3D('',#38244,#24030,#24031);
#19535=AXIS2_PLACEMENT_3D('',#38247,#24034,#24035);
#19536=AXIS2_PLACEMENT_3D('',#38250,#24038,#24039);
#19537=AXIS2_PLACEMENT_3D('',#38253,#24042,#24043);
#19538=AXIS2_PLACEMENT_3D('',#38256,#24046,#24047);
#19539=AXIS2_PLACEMENT_3D('',#38259,#24050,#24051);
#19540=AXIS2_PLACEMENT_3D('',#38262,#24054,#24055);
#19541=AXIS2_PLACEMENT_3D('',#38265,#24058,#24059);
#19542=AXIS2_PLACEMENT_3D('',#38268,#24062,#24063);
#19543=AXIS2_PLACEMENT_3D('',#38271,#24066,#24067);
#19544=AXIS2_PLACEMENT_3D('',#38274,#24070,#24071);
#19545=AXIS2_PLACEMENT_3D('',#38277,#24074,#24075);
#19546=AXIS2_PLACEMENT_3D('',#38280,#24078,#24079);
#19547=AXIS2_PLACEMENT_3D('',#38283,#24082,#24083);
#19548=AXIS2_PLACEMENT_3D('',#38286,#24086,#24087);
#19549=AXIS2_PLACEMENT_3D('',#38289,#24090,#24091);
#19550=AXIS2_PLACEMENT_3D('',#38292,#24094,#24095);
#19551=AXIS2_PLACEMENT_3D('',#38295,#24098,#24099);
#19552=AXIS2_PLACEMENT_3D('',#38298,#24102,#24103);
#19553=AXIS2_PLACEMENT_3D('',#38301,#24106,#24107);
#19554=AXIS2_PLACEMENT_3D('',#38304,#24110,#24111);
#19555=AXIS2_PLACEMENT_3D('',#38307,#24114,#24115);
#19556=AXIS2_PLACEMENT_3D('',#38310,#24118,#24119);
#19557=AXIS2_PLACEMENT_3D('',#38313,#24122,#24123);
#19558=AXIS2_PLACEMENT_3D('',#38316,#24126,#24127);
#19559=AXIS2_PLACEMENT_3D('',#38319,#24130,#24131);
#19560=AXIS2_PLACEMENT_3D('',#38322,#24134,#24135);
#19561=AXIS2_PLACEMENT_3D('',#38325,#24138,#24139);
#19562=AXIS2_PLACEMENT_3D('',#38328,#24142,#24143);
#19563=AXIS2_PLACEMENT_3D('',#38331,#24146,#24147);
#19564=AXIS2_PLACEMENT_3D('',#38334,#24150,#24151);
#19565=AXIS2_PLACEMENT_3D('',#38337,#24154,#24155);
#19566=AXIS2_PLACEMENT_3D('',#38340,#24158,#24159);
#19567=AXIS2_PLACEMENT_3D('',#38343,#24162,#24163);
#19568=AXIS2_PLACEMENT_3D('',#38346,#24166,#24167);
#19569=AXIS2_PLACEMENT_3D('',#38349,#24170,#24171);
#19570=AXIS2_PLACEMENT_3D('',#38352,#24174,#24175);
#19571=AXIS2_PLACEMENT_3D('',#38353,#24176,#24177);
#19572=AXIS2_PLACEMENT_3D('',#38356,#24180,#24181);
#19573=AXIS2_PLACEMENT_3D('',#38357,#24182,#24183);
#19574=AXIS2_PLACEMENT_3D('',#38358,#24184,#24185);
#19575=AXIS2_PLACEMENT_3D('',#38359,#24186,#24187);
#19576=AXIS2_PLACEMENT_3D('',#38361,#24189,#24190);
#19577=AXIS2_PLACEMENT_3D('',#38362,#24191,#24192);
#19578=AXIS2_PLACEMENT_3D('',#38364,#24194,#24195);
#19579=AXIS2_PLACEMENT_3D('',#38365,#24196,#24197);
#19580=AXIS2_PLACEMENT_3D('',#38367,#24199,#24200);
#19581=AXIS2_PLACEMENT_3D('',#38368,#24201,#24202);
#19582=AXIS2_PLACEMENT_3D('',#38370,#24204,#24205);
#19583=AXIS2_PLACEMENT_3D('',#38371,#24206,#24207);
#19584=AXIS2_PLACEMENT_3D('',#38373,#24209,#24210);
#19585=AXIS2_PLACEMENT_3D('',#38374,#24211,#24212);
#19586=AXIS2_PLACEMENT_3D('',#38376,#24214,#24215);
#19587=AXIS2_PLACEMENT_3D('',#38377,#24216,#24217);
#19588=AXIS2_PLACEMENT_3D('',#38379,#24219,#24220);
#19589=AXIS2_PLACEMENT_3D('',#38380,#24221,#24222);
#19590=AXIS2_PLACEMENT_3D('',#38382,#24224,#24225);
#19591=AXIS2_PLACEMENT_3D('',#38383,#24226,#24227);
#19592=AXIS2_PLACEMENT_3D('',#38385,#24229,#24230);
#19593=AXIS2_PLACEMENT_3D('',#38386,#24231,#24232);
#19594=AXIS2_PLACEMENT_3D('',#38388,#24234,#24235);
#19595=AXIS2_PLACEMENT_3D('',#38389,#24236,#24237);
#19596=AXIS2_PLACEMENT_3D('',#38391,#24239,#24240);
#19597=AXIS2_PLACEMENT_3D('',#38392,#24241,#24242);
#19598=AXIS2_PLACEMENT_3D('',#38394,#24244,#24245);
#19599=AXIS2_PLACEMENT_3D('',#38395,#24246,#24247);
#19600=AXIS2_PLACEMENT_3D('',#38397,#24249,#24250);
#19601=AXIS2_PLACEMENT_3D('',#38398,#24251,#24252);
#19602=AXIS2_PLACEMENT_3D('',#38400,#24254,#24255);
#19603=AXIS2_PLACEMENT_3D('',#38401,#24256,#24257);
#19604=AXIS2_PLACEMENT_3D('',#38403,#24259,#24260);
#19605=AXIS2_PLACEMENT_3D('',#38404,#24261,#24262);
#19606=AXIS2_PLACEMENT_3D('',#38406,#24264,#24265);
#19607=AXIS2_PLACEMENT_3D('',#38407,#24266,#24267);
#19608=AXIS2_PLACEMENT_3D('',#38409,#24269,#24270);
#19609=AXIS2_PLACEMENT_3D('',#38410,#24271,#24272);
#19610=AXIS2_PLACEMENT_3D('',#38412,#24274,#24275);
#19611=AXIS2_PLACEMENT_3D('',#38413,#24276,#24277);
#19612=AXIS2_PLACEMENT_3D('',#38415,#24279,#24280);
#19613=AXIS2_PLACEMENT_3D('',#38416,#24281,#24282);
#19614=AXIS2_PLACEMENT_3D('',#38418,#24284,#24285);
#19615=AXIS2_PLACEMENT_3D('',#38419,#24286,#24287);
#19616=AXIS2_PLACEMENT_3D('',#38421,#24289,#24290);
#19617=AXIS2_PLACEMENT_3D('',#38422,#24291,#24292);
#19618=AXIS2_PLACEMENT_3D('',#38424,#24294,#24295);
#19619=AXIS2_PLACEMENT_3D('',#38425,#24296,#24297);
#19620=AXIS2_PLACEMENT_3D('',#38427,#24299,#24300);
#19621=AXIS2_PLACEMENT_3D('',#38428,#24301,#24302);
#19622=AXIS2_PLACEMENT_3D('',#38430,#24304,#24305);
#19623=AXIS2_PLACEMENT_3D('',#38431,#24306,#24307);
#19624=AXIS2_PLACEMENT_3D('',#38433,#24309,#24310);
#19625=AXIS2_PLACEMENT_3D('',#38434,#24311,#24312);
#19626=AXIS2_PLACEMENT_3D('',#38436,#24314,#24315);
#19627=AXIS2_PLACEMENT_3D('',#38437,#24316,#24317);
#19628=AXIS2_PLACEMENT_3D('',#38439,#24319,#24320);
#19629=AXIS2_PLACEMENT_3D('',#38440,#24321,#24322);
#19630=AXIS2_PLACEMENT_3D('',#38442,#24324,#24325);
#19631=AXIS2_PLACEMENT_3D('',#38443,#24326,#24327);
#19632=AXIS2_PLACEMENT_3D('',#38445,#24329,#24330);
#19633=AXIS2_PLACEMENT_3D('',#38446,#24331,#24332);
#19634=AXIS2_PLACEMENT_3D('',#38448,#24334,#24335);
#19635=AXIS2_PLACEMENT_3D('',#38449,#24336,#24337);
#19636=AXIS2_PLACEMENT_3D('',#38451,#24339,#24340);
#19637=AXIS2_PLACEMENT_3D('',#38452,#24341,#24342);
#19638=AXIS2_PLACEMENT_3D('',#38454,#24344,#24345);
#19639=AXIS2_PLACEMENT_3D('',#38455,#24346,#24347);
#19640=AXIS2_PLACEMENT_3D('',#38457,#24349,#24350);
#19641=AXIS2_PLACEMENT_3D('',#38458,#24351,#24352);
#19642=AXIS2_PLACEMENT_3D('',#38460,#24354,#24355);
#19643=AXIS2_PLACEMENT_3D('',#38461,#24356,#24357);
#19644=AXIS2_PLACEMENT_3D('',#38463,#24359,#24360);
#19645=AXIS2_PLACEMENT_3D('',#38464,#24361,#24362);
#19646=AXIS2_PLACEMENT_3D('',#38466,#24364,#24365);
#19647=AXIS2_PLACEMENT_3D('',#38467,#24366,#24367);
#19648=AXIS2_PLACEMENT_3D('',#38469,#24369,#24370);
#19649=AXIS2_PLACEMENT_3D('',#38470,#24371,#24372);
#19650=AXIS2_PLACEMENT_3D('',#38472,#24374,#24375);
#19651=AXIS2_PLACEMENT_3D('',#38473,#24376,#24377);
#19652=AXIS2_PLACEMENT_3D('',#38475,#24379,#24380);
#19653=AXIS2_PLACEMENT_3D('',#38476,#24381,#24382);
#19654=AXIS2_PLACEMENT_3D('',#38478,#24384,#24385);
#19655=AXIS2_PLACEMENT_3D('',#38479,#24386,#24387);
#19656=AXIS2_PLACEMENT_3D('',#38481,#24389,#24390);
#19657=AXIS2_PLACEMENT_3D('',#38482,#24391,#24392);
#19658=AXIS2_PLACEMENT_3D('',#38484,#24394,#24395);
#19659=AXIS2_PLACEMENT_3D('',#38485,#24396,#24397);
#19660=AXIS2_PLACEMENT_3D('',#38487,#24399,#24400);
#19661=AXIS2_PLACEMENT_3D('',#38488,#24401,#24402);
#19662=AXIS2_PLACEMENT_3D('',#38490,#24404,#24405);
#19663=AXIS2_PLACEMENT_3D('',#38491,#24406,#24407);
#19664=AXIS2_PLACEMENT_3D('',#38493,#24409,#24410);
#19665=AXIS2_PLACEMENT_3D('',#38494,#24411,#24412);
#19666=AXIS2_PLACEMENT_3D('',#38496,#24414,#24415);
#19667=AXIS2_PLACEMENT_3D('',#38497,#24416,#24417);
#19668=AXIS2_PLACEMENT_3D('',#38499,#24419,#24420);
#19669=AXIS2_PLACEMENT_3D('',#38500,#24421,#24422);
#19670=AXIS2_PLACEMENT_3D('',#38502,#24424,#24425);
#19671=AXIS2_PLACEMENT_3D('',#38503,#24426,#24427);
#19672=AXIS2_PLACEMENT_3D('',#38505,#24429,#24430);
#19673=AXIS2_PLACEMENT_3D('',#38506,#24431,#24432);
#19674=AXIS2_PLACEMENT_3D('',#38508,#24434,#24435);
#19675=AXIS2_PLACEMENT_3D('',#38509,#24436,#24437);
#19676=AXIS2_PLACEMENT_3D('',#38511,#24439,#24440);
#19677=AXIS2_PLACEMENT_3D('',#38512,#24441,#24442);
#19678=AXIS2_PLACEMENT_3D('',#38514,#24444,#24445);
#19679=AXIS2_PLACEMENT_3D('',#38515,#24446,#24447);
#19680=AXIS2_PLACEMENT_3D('',#38517,#24449,#24450);
#19681=AXIS2_PLACEMENT_3D('',#38518,#24451,#24452);
#19682=AXIS2_PLACEMENT_3D('',#38520,#24454,#24455);
#19683=AXIS2_PLACEMENT_3D('',#38521,#24456,#24457);
#19684=AXIS2_PLACEMENT_3D('',#38523,#24459,#24460);
#19685=AXIS2_PLACEMENT_3D('',#38524,#24461,#24462);
#19686=AXIS2_PLACEMENT_3D('',#38526,#24464,#24465);
#19687=AXIS2_PLACEMENT_3D('',#38527,#24466,#24467);
#19688=AXIS2_PLACEMENT_3D('',#38529,#24469,#24470);
#19689=AXIS2_PLACEMENT_3D('',#38530,#24471,#24472);
#19690=AXIS2_PLACEMENT_3D('',#38532,#24474,#24475);
#19691=AXIS2_PLACEMENT_3D('',#38533,#24476,#24477);
#19692=AXIS2_PLACEMENT_3D('',#38535,#24479,#24480);
#19693=AXIS2_PLACEMENT_3D('',#38536,#24481,#24482);
#19694=AXIS2_PLACEMENT_3D('',#38538,#24484,#24485);
#19695=AXIS2_PLACEMENT_3D('',#38539,#24486,#24487);
#19696=AXIS2_PLACEMENT_3D('',#38541,#24489,#24490);
#19697=AXIS2_PLACEMENT_3D('',#38542,#24491,#24492);
#19698=AXIS2_PLACEMENT_3D('',#38544,#24494,#24495);
#19699=AXIS2_PLACEMENT_3D('',#38545,#24496,#24497);
#19700=AXIS2_PLACEMENT_3D('',#38547,#24499,#24500);
#19701=AXIS2_PLACEMENT_3D('',#38548,#24501,#24502);
#19702=AXIS2_PLACEMENT_3D('',#38550,#24504,#24505);
#19703=AXIS2_PLACEMENT_3D('',#38551,#24506,#24507);
#19704=AXIS2_PLACEMENT_3D('',#38553,#24509,#24510);
#19705=AXIS2_PLACEMENT_3D('',#38554,#24511,#24512);
#19706=AXIS2_PLACEMENT_3D('',#38556,#24514,#24515);
#19707=AXIS2_PLACEMENT_3D('',#38557,#24516,#24517);
#19708=AXIS2_PLACEMENT_3D('',#38559,#24519,#24520);
#19709=AXIS2_PLACEMENT_3D('',#38560,#24521,#24522);
#19710=AXIS2_PLACEMENT_3D('',#38562,#24524,#24525);
#19711=AXIS2_PLACEMENT_3D('',#38563,#24526,#24527);
#19712=AXIS2_PLACEMENT_3D('',#38565,#24529,#24530);
#19713=AXIS2_PLACEMENT_3D('',#38566,#24531,#24532);
#19714=AXIS2_PLACEMENT_3D('',#38568,#24534,#24535);
#19715=AXIS2_PLACEMENT_3D('',#38569,#24536,#24537);
#19716=AXIS2_PLACEMENT_3D('',#38571,#24539,#24540);
#19717=AXIS2_PLACEMENT_3D('',#38572,#24541,#24542);
#19718=AXIS2_PLACEMENT_3D('',#38574,#24544,#24545);
#19719=AXIS2_PLACEMENT_3D('',#38575,#24546,#24547);
#19720=AXIS2_PLACEMENT_3D('',#38577,#24549,#24550);
#19721=AXIS2_PLACEMENT_3D('',#38578,#24551,#24552);
#19722=AXIS2_PLACEMENT_3D('',#38580,#24554,#24555);
#19723=AXIS2_PLACEMENT_3D('',#38581,#24556,#24557);
#19724=AXIS2_PLACEMENT_3D('',#38583,#24559,#24560);
#19725=AXIS2_PLACEMENT_3D('',#38584,#24561,#24562);
#19726=AXIS2_PLACEMENT_3D('',#38586,#24564,#24565);
#19727=AXIS2_PLACEMENT_3D('',#38587,#24566,#24567);
#19728=AXIS2_PLACEMENT_3D('',#38589,#24569,#24570);
#19729=AXIS2_PLACEMENT_3D('',#38590,#24571,#24572);
#19730=AXIS2_PLACEMENT_3D('',#38591,#24573,#24574);
#19731=AXIS2_PLACEMENT_3D('',#38592,#24575,#24576);
#19732=AXIS2_PLACEMENT_3D('',#38593,#24577,#24578);
#19733=AXIS2_PLACEMENT_3D('',#38594,#24579,#24580);
#19734=AXIS2_PLACEMENT_3D('',#38595,#24581,#24582);
#19735=AXIS2_PLACEMENT_3D('',#38596,#24583,#24584);
#19736=AXIS2_PLACEMENT_3D('',#38597,#24585,#24586);
#19737=AXIS2_PLACEMENT_3D('',#38598,#24587,#24588);
#19738=AXIS2_PLACEMENT_3D('',#38599,#24589,#24590);
#19739=AXIS2_PLACEMENT_3D('',#38600,#24591,#24592);
#19740=AXIS2_PLACEMENT_3D('',#38601,#24593,#24594);
#19741=AXIS2_PLACEMENT_3D('',#38602,#24595,#24596);
#19742=AXIS2_PLACEMENT_3D('',#38603,#24597,#24598);
#19743=DIRECTION('axis',(0.,0.,1.));
#19744=DIRECTION('refdir',(1.,0.,0.));
#19745=DIRECTION('axis',(0.,0.,1.));
#19746=DIRECTION('refdir',(1.,0.,0.));
#19747=DIRECTION('center_axis',(0.,1.,0.));
#19748=DIRECTION('ref_axis',(0.,0.,1.));
#19749=DIRECTION('center_axis',(0.,1.,0.));
#19750=DIRECTION('ref_axis',(0.,0.,1.));
#19751=DIRECTION('',(0.,1.,0.));
#19752=DIRECTION('center_axis',(0.,1.,0.));
#19753=DIRECTION('ref_axis',(0.,0.,1.));
#19754=DIRECTION('',(0.,-1.,0.));
#19755=DIRECTION('center_axis',(0.,-1.,0.));
#19756=DIRECTION('ref_axis',(1.22464679914735E-16,0.,1.));
#19757=DIRECTION('center_axis',(0.,-1.,0.));
#19758=DIRECTION('ref_axis',(0.,0.,-1.));
#19759=DIRECTION('',(0.,1.,0.));
#19760=DIRECTION('center_axis',(0.,1.,0.));
#19761=DIRECTION('ref_axis',(0.,0.,1.));
#19762=DIRECTION('',(0.,-1.,0.));
#19763=DIRECTION('center_axis',(0.,0.,1.));
#19764=DIRECTION('ref_axis',(1.,0.,0.));
#19765=DIRECTION('',(1.,0.,0.));
#19766=DIRECTION('',(0.,1.,0.));
#19767=DIRECTION('',(1.,0.,0.));
#19768=DIRECTION('',(0.,1.,0.));
#19769=DIRECTION('',(1.,0.,0.));
#19770=DIRECTION('',(-1.,0.,0.));
#19771=DIRECTION('center_axis',(0.,0.,1.));
#19772=DIRECTION('ref_axis',(1.,0.,0.));
#19773=DIRECTION('',(1.,0.,0.));
#19774=DIRECTION('',(-1.,0.,0.));
#19775=DIRECTION('',(1.,0.,0.));
#19776=DIRECTION('',(0.,-1.,0.));
#19777=DIRECTION('',(1.,0.,0.));
#19778=DIRECTION('',(0.,-1.,0.));
#19779=DIRECTION('center_axis',(0.,1.,0.));
#19780=DIRECTION('ref_axis',(0.,0.,1.));
#19781=DIRECTION('center_axis',(0.,-1.,0.));
#19782=DIRECTION('ref_axis',(0.,0.,-1.));
#19783=DIRECTION('center_axis',(0.,1.,0.));
#19784=DIRECTION('ref_axis',(0.,0.,1.));
#19785=DIRECTION('center_axis',(0.,1.,0.));
#19786=DIRECTION('ref_axis',(0.,0.,1.));
#19787=DIRECTION('center_axis',(0.,1.,0.));
#19788=DIRECTION('ref_axis',(0.,0.,1.));
#19789=DIRECTION('center_axis',(0.,-1.,0.));
#19790=DIRECTION('ref_axis',(-1.22464679914735E-16,0.,1.));
#19791=DIRECTION('center_axis',(0.,1.,0.));
#19792=DIRECTION('ref_axis',(0.,0.,1.));
#19793=DIRECTION('center_axis',(0.,-1.,0.));
#19794=DIRECTION('ref_axis',(0.,0.,-1.));
#19795=DIRECTION('center_axis',(0.,-1.,0.));
#19796=DIRECTION('ref_axis',(0.,0.,-1.));
#19797=DIRECTION('center_axis',(0.,-1.,0.));
#19798=DIRECTION('ref_axis',(1.22464679914735E-16,0.,1.));
#19799=DIRECTION('center_axis',(0.,-1.,0.));
#19800=DIRECTION('ref_axis',(0.,0.,-1.));
#19801=DIRECTION('center_axis',(0.,-1.,0.));
#19802=DIRECTION('ref_axis',(0.,0.,-1.));
#19803=DIRECTION('',(0.,-1.,0.));
#19804=DIRECTION('center_axis',(0.,1.,0.));
#19805=DIRECTION('ref_axis',(0.,0.,1.));
#19806=DIRECTION('',(0.,1.,0.));
#19807=DIRECTION('center_axis',(0.,-1.,0.));
#19808=DIRECTION('ref_axis',(0.,0.,-1.));
#19809=DIRECTION('center_axis',(0.,1.,0.));
#19810=DIRECTION('ref_axis',(0.,0.,1.));
#19811=DIRECTION('',(0.,1.,0.));
#19812=DIRECTION('center_axis',(0.,1.,0.));
#19813=DIRECTION('ref_axis',(0.,0.,1.));
#19814=DIRECTION('',(0.,-1.,0.));
#19815=DIRECTION('center_axis',(0.,-1.,0.));
#19816=DIRECTION('ref_axis',(0.,0.,-1.));
#19817=DIRECTION('center_axis',(0.,1.,0.));
#19818=DIRECTION('ref_axis',(0.,0.,1.));
#19819=DIRECTION('',(0.,-1.,0.));
#19820=DIRECTION('center_axis',(0.,-1.,0.));
#19821=DIRECTION('ref_axis',(0.,0.,-1.));
#19822=DIRECTION('',(0.,1.,0.));
#19823=DIRECTION('center_axis',(0.,0.,-1.));
#19824=DIRECTION('ref_axis',(-1.,0.,0.));
#19825=DIRECTION('',(-1.,0.,0.));
#19826=DIRECTION('',(-1.,0.,0.));
#19827=DIRECTION('',(-1.,0.,0.));
#19828=DIRECTION('',(0.,1.,0.));
#19829=DIRECTION('',(1.,0.,0.));
#19830=DIRECTION('center_axis',(0.,0.,-1.));
#19831=DIRECTION('ref_axis',(-1.,0.,0.));
#19832=DIRECTION('',(-1.,0.,0.));
#19833=DIRECTION('',(1.,0.,0.));
#19834=DIRECTION('',(0.,-1.,0.));
#19835=DIRECTION('',(-1.,0.,0.));
#19836=DIRECTION('',(-1.,0.,0.));
#19837=DIRECTION('center_axis',(0.,1.,0.));
#19838=DIRECTION('ref_axis',(0.,0.,1.));
#19839=DIRECTION('center_axis',(0.,1.,0.));
#19840=DIRECTION('ref_axis',(0.,0.,1.));
#19841=DIRECTION('center_axis',(0.,1.,0.));
#19842=DIRECTION('ref_axis',(0.,0.,1.));
#19843=DIRECTION('center_axis',(0.,1.,0.));
#19844=DIRECTION('ref_axis',(0.,0.,1.));
#19845=DIRECTION('center_axis',(0.,1.,0.));
#19846=DIRECTION('ref_axis',(0.,0.,1.));
#19847=DIRECTION('center_axis',(0.,1.,0.));
#19848=DIRECTION('ref_axis',(-1.22464679914735E-16,0.,-1.));
#19849=DIRECTION('center_axis',(0.,-1.,0.));
#19850=DIRECTION('ref_axis',(0.,0.,-1.));
#19851=DIRECTION('center_axis',(1.,0.,0.));
#19852=DIRECTION('ref_axis',(0.,0.,-1.));
#19853=DIRECTION('',(0.,1.,0.));
#19854=DIRECTION('',(0.,0.,-1.));
#19855=DIRECTION('',(0.,1.,0.));
#19856=DIRECTION('',(0.,0.,1.));
#19857=DIRECTION('center_axis',(0.,0.,1.));
#19858=DIRECTION('ref_axis',(1.,0.,0.));
#19859=DIRECTION('',(0.,1.,0.));
#19860=DIRECTION('',(1.,0.,0.));
#19861=DIRECTION('',(-1.,0.,0.));
#19862=DIRECTION('',(0.,1.,0.));
#19863=DIRECTION('',(1.,0.,0.));
#19864=DIRECTION('',(0.,1.,0.));
#19865=DIRECTION('',(1.,0.,0.));
#19866=DIRECTION('center_axis',(0.,0.,-1.));
#19867=DIRECTION('ref_axis',(-1.,0.,0.));
#19868=DIRECTION('',(-1.,0.,0.));
#19869=DIRECTION('',(0.,-1.,0.));
#19870=DIRECTION('',(-1.,0.,0.));
#19871=DIRECTION('',(0.,1.,0.));
#19872=DIRECTION('',(-1.,0.,0.));
#19873=DIRECTION('',(0.,-1.,0.));
#19874=DIRECTION('',(1.,0.,0.));
#19875=DIRECTION('center_axis',(0.,1.,0.));
#19876=DIRECTION('ref_axis',(0.,0.,1.));
#19877=DIRECTION('center_axis',(0.,-1.,0.));
#19878=DIRECTION('ref_axis',(0.,0.,-1.));
#19879=DIRECTION('center_axis',(0.,-1.,0.));
#19880=DIRECTION('ref_axis',(0.,0.,1.));
#19881=DIRECTION('center_axis',(0.,1.,0.));
#19882=DIRECTION('ref_axis',(0.,0.,1.));
#19883=DIRECTION('center_axis',(0.,1.,0.));
#19884=DIRECTION('ref_axis',(0.,0.,1.));
#19885=DIRECTION('center_axis',(0.,-1.,0.));
#19886=DIRECTION('ref_axis',(0.,0.,1.));
#19887=DIRECTION('center_axis',(0.,1.,0.));
#19888=DIRECTION('ref_axis',(0.,0.,1.));
#19889=DIRECTION('center_axis',(0.,1.,0.));
#19890=DIRECTION('ref_axis',(0.,0.,1.));
#19891=DIRECTION('center_axis',(0.,1.,0.));
#19892=DIRECTION('ref_axis',(0.,0.,1.));
#19893=DIRECTION('center_axis',(0.,1.,0.));
#19894=DIRECTION('ref_axis',(0.,0.,1.));
#19895=DIRECTION('center_axis',(0.,-1.,0.));
#19896=DIRECTION('ref_axis',(0.,0.,-1.));
#19897=DIRECTION('center_axis',(0.,-1.,0.));
#19898=DIRECTION('ref_axis',(0.,0.,-1.));
#19899=DIRECTION('center_axis',(0.,-1.,0.));
#19900=DIRECTION('ref_axis',(0.,0.,-1.));
#19901=DIRECTION('center_axis',(-1.,0.,0.));
#19902=DIRECTION('ref_axis',(0.,0.,1.));
#19903=DIRECTION('',(0.,1.,0.));
#19904=DIRECTION('',(0.,0.,1.));
#19905=DIRECTION('',(0.,1.,0.));
#19906=DIRECTION('',(0.,0.,-1.));
#19907=DIRECTION('center_axis',(0.,0.,-1.));
#19908=DIRECTION('ref_axis',(-1.,0.,0.));
#19909=DIRECTION('',(0.,1.,0.));
#19910=DIRECTION('',(-1.,0.,0.));
#19911=DIRECTION('',(1.,0.,0.));
#19912=DIRECTION('',(0.,1.,0.));
#19913=DIRECTION('',(-1.,0.,0.));
#19914=DIRECTION('',(0.,1.,0.));
#19915=DIRECTION('',(-1.,0.,0.));
#19916=DIRECTION('center_axis',(0.,0.,1.));
#19917=DIRECTION('ref_axis',(1.,0.,0.));
#19918=DIRECTION('',(1.,0.,0.));
#19919=DIRECTION('',(0.,-1.,0.));
#19920=DIRECTION('',(1.,0.,0.));
#19921=DIRECTION('',(0.,1.,0.));
#19922=DIRECTION('',(1.,0.,0.));
#19923=DIRECTION('',(0.,-1.,0.));
#19924=DIRECTION('',(-1.,0.,0.));
#19925=DIRECTION('center_axis',(0.,1.,0.));
#19926=DIRECTION('ref_axis',(0.,0.,1.));
#19927=DIRECTION('center_axis',(0.,-1.,0.));
#19928=DIRECTION('ref_axis',(0.,0.,-1.));
#19929=DIRECTION('center_axis',(0.,-1.,0.));
#19930=DIRECTION('ref_axis',(0.,0.,1.));
#19931=DIRECTION('center_axis',(0.,1.,0.));
#19932=DIRECTION('ref_axis',(0.,0.,1.));
#19933=DIRECTION('center_axis',(0.,1.,0.));
#19934=DIRECTION('ref_axis',(0.,0.,1.));
#19935=DIRECTION('center_axis',(0.,-1.,0.));
#19936=DIRECTION('ref_axis',(0.,0.,1.));
#19937=DIRECTION('center_axis',(0.,1.,0.));
#19938=DIRECTION('ref_axis',(0.,0.,1.));
#19939=DIRECTION('center_axis',(0.,1.,0.));
#19940=DIRECTION('ref_axis',(0.,0.,1.));
#19941=DIRECTION('center_axis',(0.,1.,0.));
#19942=DIRECTION('ref_axis',(0.,0.,1.));
#19943=DIRECTION('center_axis',(0.,1.,0.));
#19944=DIRECTION('ref_axis',(0.,0.,1.));
#19945=DIRECTION('center_axis',(0.,-1.,0.));
#19946=DIRECTION('ref_axis',(0.,0.,-1.));
#19947=DIRECTION('center_axis',(0.,-1.,0.));
#19948=DIRECTION('ref_axis',(0.,0.,-1.));
#19949=DIRECTION('center_axis',(0.,-1.,0.));
#19950=DIRECTION('ref_axis',(0.,0.,-1.));
#19951=DIRECTION('axis',(0.,0.,1.));
#19952=DIRECTION('refdir',(1.,0.,0.));
#19953=DIRECTION('center_axis',(0.,-1.,0.));
#19954=DIRECTION('ref_axis',(1.22464679914735E-16,0.,1.));
#19955=DIRECTION('center_axis',(0.,-1.,0.));
#19956=DIRECTION('ref_axis',(0.,0.,-1.));
#19957=DIRECTION('',(0.,1.,0.));
#19958=DIRECTION('center_axis',(0.,1.,0.));
#19959=DIRECTION('ref_axis',(0.,0.,1.));
#19960=DIRECTION('',(0.,-1.,0.));
#19961=DIRECTION('center_axis',(0.,1.,0.));
#19962=DIRECTION('ref_axis',(0.,0.,1.));
#19963=DIRECTION('center_axis',(0.,-1.,0.));
#19964=DIRECTION('ref_axis',(0.,0.,-1.));
#19965=DIRECTION('',(1.,0.,0.));
#19966=DIRECTION('center_axis',(0.,0.,1.));
#19967=DIRECTION('ref_axis',(1.,0.,0.));
#19968=DIRECTION('',(1.,0.,0.));
#19969=DIRECTION('',(1.,0.,0.));
#19970=DIRECTION('',(1.,0.,0.));
#19971=DIRECTION('',(0.,1.,0.));
#19972=DIRECTION('',(0.,-1.,0.));
#19973=DIRECTION('center_axis',(0.,1.,0.));
#19974=DIRECTION('ref_axis',(0.,0.,1.));
#19975=DIRECTION('center_axis',(0.,-1.,0.));
#19976=DIRECTION('ref_axis',(0.,0.,-1.));
#19977=DIRECTION('center_axis',(0.,-1.,0.));
#19978=DIRECTION('ref_axis',(0.,0.,-1.));
#19979=DIRECTION('center_axis',(0.,-1.,0.));
#19980=DIRECTION('ref_axis',(-1.22464679914735E-16,0.,1.));
#19981=DIRECTION('center_axis',(0.,-1.,0.));
#19982=DIRECTION('ref_axis',(0.,0.,-1.));
#19983=DIRECTION('center_axis',(0.,-1.,0.));
#19984=DIRECTION('ref_axis',(0.,0.,-1.));
#19985=DIRECTION('',(0.,-1.,0.));
#19986=DIRECTION('center_axis',(0.,-1.,0.));
#19987=DIRECTION('ref_axis',(0.,0.,-1.));
#19988=DIRECTION('',(0.,1.,0.));
#19989=DIRECTION('center_axis',(0.,-1.,0.));
#19990=DIRECTION('ref_axis',(0.,0.,-1.));
#19991=DIRECTION('center_axis',(0.,1.,0.));
#19992=DIRECTION('ref_axis',(0.,0.,1.));
#19993=DIRECTION('',(0.,-1.,0.));
#19994=DIRECTION('center_axis',(0.,-1.,0.));
#19995=DIRECTION('ref_axis',(0.,0.,-1.));
#19996=DIRECTION('',(0.,1.,0.));
#19997=DIRECTION('center_axis',(0.,1.,0.));
#19998=DIRECTION('ref_axis',(0.,0.,1.));
#19999=DIRECTION('',(-1.,0.,0.));
#20000=DIRECTION('center_axis',(0.,0.,-1.));
#20001=DIRECTION('ref_axis',(-1.,0.,0.));
#20002=DIRECTION('',(-1.,0.,0.));
#20003=DIRECTION('',(-1.,0.,0.));
#20004=DIRECTION('',(-1.,0.,0.));
#20005=DIRECTION('center_axis',(0.,1.,0.));
#20006=DIRECTION('ref_axis',(0.,0.,1.));
#20007=DIRECTION('center_axis',(0.,-1.,0.));
#20008=DIRECTION('ref_axis',(0.,0.,-1.));
#20009=DIRECTION('center_axis',(1.,0.,0.));
#20010=DIRECTION('ref_axis',(0.,0.,-1.));
#20011=DIRECTION('',(0.,1.,0.));
#20012=DIRECTION('',(0.,0.,-1.));
#20013=DIRECTION('',(0.,1.,0.));
#20014=DIRECTION('',(0.,0.,-1.));
#20015=DIRECTION('center_axis',(0.,0.,1.));
#20016=DIRECTION('ref_axis',(1.,0.,0.));
#20017=DIRECTION('',(0.,1.,0.));
#20018=DIRECTION('',(1.,0.,0.));
#20019=DIRECTION('',(0.,-1.,0.));
#20020=DIRECTION('',(1.,0.,0.));
#20021=DIRECTION('',(0.,1.,0.));
#20022=DIRECTION('',(1.,0.,0.));
#20023=DIRECTION('',(1.,0.,0.));
#20024=DIRECTION('center_axis',(-1.,0.,0.));
#20025=DIRECTION('ref_axis',(0.,0.,1.));
#20026=DIRECTION('',(0.,1.,0.));
#20027=DIRECTION('',(0.,0.,1.));
#20028=DIRECTION('',(0.,0.,1.));
#20029=DIRECTION('center_axis',(0.,0.,-1.));
#20030=DIRECTION('ref_axis',(-1.,0.,0.));
#20031=DIRECTION('',(-1.,0.,0.));
#20032=DIRECTION('',(0.,-1.,0.));
#20033=DIRECTION('',(-1.,0.,0.));
#20034=DIRECTION('',(0.,1.,0.));
#20035=DIRECTION('',(-1.,0.,0.));
#20036=DIRECTION('',(-1.,0.,0.));
#20037=DIRECTION('center_axis',(0.,-1.,0.));
#20038=DIRECTION('ref_axis',(0.,0.,-1.));
#20039=DIRECTION('center_axis',(0.,-1.,0.));
#20040=DIRECTION('ref_axis',(0.,0.,-1.));
#20041=DIRECTION('center_axis',(0.,-1.,0.));
#20042=DIRECTION('ref_axis',(0.,0.,-1.));
#20043=DIRECTION('center_axis',(0.,-1.,0.));
#20044=DIRECTION('ref_axis',(0.,0.,-1.));
#20045=DIRECTION('center_axis',(0.,-1.,0.));
#20046=DIRECTION('ref_axis',(0.,0.,-1.));
#20047=DIRECTION('center_axis',(0.,-1.,0.));
#20048=DIRECTION('ref_axis',(0.,0.,-1.));
#20049=DIRECTION('center_axis',(0.,-1.,0.));
#20050=DIRECTION('ref_axis',(0.,0.,-1.));
#20051=DIRECTION('center_axis',(0.,-1.,0.));
#20052=DIRECTION('ref_axis',(0.,0.,-1.));
#20053=DIRECTION('center_axis',(0.,-1.,0.));
#20054=DIRECTION('ref_axis',(0.,0.,-1.));
#20055=DIRECTION('center_axis',(0.,-1.,0.));
#20056=DIRECTION('ref_axis',(0.,0.,-1.));
#20057=DIRECTION('center_axis',(-0.91945378174003,0.,-0.39319809669422));
#20058=DIRECTION('ref_axis',(-0.39319809669422,0.,0.91945378174003));
#20059=DIRECTION('',(-0.136517154531564,-1.04972719113862E-16,-0.990637706994139));
#20060=DIRECTION('center_axis',(-0.91945378174003,0.,-0.39319809669422));
#20061=DIRECTION('ref_axis',(-0.39319809669422,0.,0.91945378174003));
#20062=DIRECTION('center_axis',(-0.91945378174003,0.,-0.39319809669422));
#20063=DIRECTION('ref_axis',(-0.39319809669422,0.,0.91945378174003));
#20064=DIRECTION('',(-0.91945378174003,0.,-0.39319809669422));
#20065=DIRECTION('center_axis',(0.,-1.,0.));
#20066=DIRECTION('ref_axis',(0.,0.,-1.));
#20067=DIRECTION('center_axis',(0.,-1.,0.));
#20068=DIRECTION('ref_axis',(0.,0.,1.));
#20069=DIRECTION('',(8.65956056235493E-17,0.707106781186548,-0.707106781186547));
#20070=DIRECTION('center_axis',(0.,1.,0.));
#20071=DIRECTION('ref_axis',(0.,0.,1.));
#20072=DIRECTION('center_axis',(0.,-1.,0.));
#20073=DIRECTION('ref_axis',(0.,0.,-1.));
#20074=DIRECTION('center_axis',(0.,-1.,0.));
#20075=DIRECTION('ref_axis',(0.,0.,-1.));
#20076=DIRECTION('center_axis',(0.,-1.,0.));
#20077=DIRECTION('ref_axis',(0.,0.,-1.));
#20078=DIRECTION('',(9.71577628780521E-17,0.608761429008721,-0.793353340291235));
#20079=DIRECTION('center_axis',(0.,1.,0.));
#20080=DIRECTION('ref_axis',(0.,0.,1.));
#20081=DIRECTION('center_axis',(0.,-1.,0.));
#20082=DIRECTION('ref_axis',(0.,0.,-1.));
#20083=DIRECTION('center_axis',(0.,1.,0.));
#20084=DIRECTION('ref_axis',(0.,0.,1.));
#20085=DIRECTION('',(0.,1.,0.));
#20086=DIRECTION('center_axis',(0.,-1.,0.));
#20087=DIRECTION('ref_axis',(0.,0.,1.));
#20088=DIRECTION('center_axis',(0.,1.,0.));
#20089=DIRECTION('ref_axis',(0.,0.,1.));
#20090=DIRECTION('',(-3.16961915143177E-17,0.965925826289068,0.258819045102521));
#20091=DIRECTION('center_axis',(0.,1.,0.));
#20092=DIRECTION('ref_axis',(0.,0.,1.));
#20093=DIRECTION('center_axis',(0.,1.,0.));
#20094=DIRECTION('ref_axis',(0.,0.,1.));
#20095=DIRECTION('center_axis',(0.,1.,0.));
#20096=DIRECTION('ref_axis',(0.,0.,1.));
#20097=DIRECTION('axis',(0.,0.,1.));
#20098=DIRECTION('refdir',(1.,0.,0.));
#20099=DIRECTION('center_axis',(1.,4.0668225646129E-15,-2.78321068817773E-14));
#20100=DIRECTION('ref_axis',(-2.89386232545955E-14,0.0348994967025012,-0.999390827019096));
#20101=DIRECTION('',(-1.,-4.0668225646129E-15,2.78321068817773E-14));
#20102=DIRECTION('',(1.,0.,-2.18547839493123E-14));
#20103=DIRECTION('center_axis',(1.,4.0668225646129E-15,-2.78321068817773E-14));
#20104=DIRECTION('ref_axis',(-2.89386232545955E-14,0.0348994967025012,-0.999390827019096));
#20105=DIRECTION('',(-1.,-4.0668225646129E-15,2.78321068817773E-14));
#20106=DIRECTION('center_axis',(1.,4.0668225646129E-15,-2.78321068817773E-14));
#20107=DIRECTION('ref_axis',(-2.89386232545955E-14,0.0348994967025012,-0.999390827019096));
#20108=DIRECTION('',(-1.,-4.0668225646129E-15,2.78321068817773E-14));
#20109=DIRECTION('center_axis',(1.,4.0668225646129E-15,-2.78321068817773E-14));
#20110=DIRECTION('ref_axis',(-2.89386232545955E-14,0.0348994967025012,-0.999390827019096));
#20111=DIRECTION('',(-1.,-4.0668225646129E-15,2.78321068817773E-14));
#20112=DIRECTION('center_axis',(1.,4.0668225646129E-15,-2.78321068817773E-14));
#20113=DIRECTION('ref_axis',(-2.89386232545955E-14,0.0348994967025012,-0.999390827019096));
#20114=DIRECTION('',(-1.,-4.0668225646129E-15,2.78321068817773E-14));
#20115=DIRECTION('center_axis',(1.,4.0668225646129E-15,-2.78321068817773E-14));
#20116=DIRECTION('ref_axis',(-2.89386232545955E-14,0.0348994967025012,-0.999390827019096));
#20117=DIRECTION('',(-1.,-4.0668225646129E-15,2.78321068817773E-14));
#20118=DIRECTION('center_axis',(1.,4.0668225646129E-15,-2.78321068817773E-14));
#20119=DIRECTION('ref_axis',(-2.89386232545955E-14,0.0348994967025012,-0.999390827019096));
#20120=DIRECTION('',(-1.,-4.0668225646129E-15,2.78321068817773E-14));
#20121=DIRECTION('center_axis',(1.,4.0668225646129E-15,-2.78321068817773E-14));
#20122=DIRECTION('ref_axis',(-2.89386232545955E-14,0.0348994967025012,-0.999390827019096));
#20123=DIRECTION('',(-1.,-4.0668225646129E-15,2.78321068817773E-14));
#20124=DIRECTION('center_axis',(1.,4.0668225646129E-15,-2.78321068817773E-14));
#20125=DIRECTION('ref_axis',(-2.89386232545955E-14,0.0348994967025012,-0.999390827019096));
#20126=DIRECTION('',(-1.,-4.0668225646129E-15,2.78321068817773E-14));
#20127=DIRECTION('center_axis',(1.,4.0668225646129E-15,-2.78321068817773E-14));
#20128=DIRECTION('ref_axis',(-2.89386232545955E-14,0.0348994967025012,-0.999390827019096));
#20129=DIRECTION('',(-1.,-4.0668225646129E-15,2.78321068817773E-14));
#20130=DIRECTION('center_axis',(1.,4.0668225646129E-15,-2.78321068817773E-14));
#20131=DIRECTION('ref_axis',(-2.89386232545955E-14,0.0348994967025012,-0.999390827019096));
#20132=DIRECTION('',(-1.,-4.0668225646129E-15,2.78321068817773E-14));
#20133=DIRECTION('center_axis',(1.,4.0668225646129E-15,-2.78321068817773E-14));
#20134=DIRECTION('ref_axis',(-2.89386232545955E-14,0.0348994967025012,-0.999390827019096));
#20135=DIRECTION('',(-1.,-4.0668225646129E-15,2.78321068817773E-14));
#20136=DIRECTION('center_axis',(1.,4.0668225646129E-15,-2.78321068817773E-14));
#20137=DIRECTION('ref_axis',(-2.89386232545955E-14,0.0348994967025012,-0.999390827019096));
#20138=DIRECTION('',(-1.,-4.0668225646129E-15,2.78321068817773E-14));
#20139=DIRECTION('center_axis',(1.,4.0668225646129E-15,-2.78321068817773E-14));
#20140=DIRECTION('ref_axis',(-2.89386232545955E-14,0.0348994967025012,-0.999390827019096));
#20141=DIRECTION('',(-1.,-4.0668225646129E-15,2.78321068817773E-14));
#20142=DIRECTION('center_axis',(1.,4.0668225646129E-15,-2.78321068817773E-14));
#20143=DIRECTION('ref_axis',(-2.89386232545955E-14,0.0348994967025012,-0.999390827019096));
#20144=DIRECTION('',(-1.,-4.0668225646129E-15,2.78321068817773E-14));
#20145=DIRECTION('center_axis',(1.,4.0668225646129E-15,-2.78321068817773E-14));
#20146=DIRECTION('ref_axis',(-2.89386232545955E-14,0.0348994967025012,-0.999390827019096));
#20147=DIRECTION('',(-1.,-4.0668225646129E-15,2.78321068817773E-14));
#20148=DIRECTION('center_axis',(1.,4.0668225646129E-15,-2.78321068817773E-14));
#20149=DIRECTION('ref_axis',(-2.89386232545955E-14,0.0348994967025012,-0.999390827019096));
#20150=DIRECTION('',(-1.,-4.0668225646129E-15,2.78321068817773E-14));
#20151=DIRECTION('center_axis',(1.,4.0668225646129E-15,-2.78321068817773E-14));
#20152=DIRECTION('ref_axis',(-2.89386232545955E-14,0.0348994967025012,-0.999390827019096));
#20153=DIRECTION('',(-1.,-4.0668225646129E-15,2.78321068817773E-14));
#20154=DIRECTION('center_axis',(1.,4.0668225646129E-15,-2.78321068817773E-14));
#20155=DIRECTION('ref_axis',(-2.89386232545955E-14,0.0348994967025012,-0.999390827019096));
#20156=DIRECTION('',(-1.,-4.0668225646129E-15,2.78321068817773E-14));
#20157=DIRECTION('center_axis',(1.,4.0668225646129E-15,-2.78321068817773E-14));
#20158=DIRECTION('ref_axis',(-2.89386232545955E-14,0.0348994967025012,-0.999390827019096));
#20159=DIRECTION('',(-1.,-4.0668225646129E-15,2.78321068817773E-14));
#20160=DIRECTION('center_axis',(1.,4.0668225646129E-15,-2.78321068817773E-14));
#20161=DIRECTION('ref_axis',(-2.89386232545955E-14,0.0348994967025012,-0.999390827019096));
#20162=DIRECTION('',(-1.,-4.0668225646129E-15,2.78321068817773E-14));
#20163=DIRECTION('center_axis',(1.,4.0668225646129E-15,-2.78321068817773E-14));
#20164=DIRECTION('ref_axis',(-2.89386232545955E-14,0.0348994967025012,-0.999390827019096));
#20165=DIRECTION('',(-1.,-4.0668225646129E-15,2.78321068817773E-14));
#20166=DIRECTION('center_axis',(1.,4.0668225646129E-15,-2.78321068817773E-14));
#20167=DIRECTION('ref_axis',(-2.89386232545955E-14,0.0348994967025012,-0.999390827019096));
#20168=DIRECTION('',(-1.,-4.0668225646129E-15,2.78321068817773E-14));
#20169=DIRECTION('center_axis',(1.,4.0668225646129E-15,-2.78321068817773E-14));
#20170=DIRECTION('ref_axis',(-2.89386232545955E-14,0.0348994967025012,-0.999390827019096));
#20171=DIRECTION('',(-1.,-4.0668225646129E-15,2.78321068817773E-14));
#20172=DIRECTION('center_axis',(1.,4.0668225646129E-15,-2.78321068817773E-14));
#20173=DIRECTION('ref_axis',(-2.89386232545955E-14,0.0348994967025012,-0.999390827019096));
#20174=DIRECTION('',(-1.,-4.0668225646129E-15,2.78321068817773E-14));
#20175=DIRECTION('center_axis',(-1.,4.23441820549806E-14,-5.91799305310465E-15));
#20176=DIRECTION('ref_axis',(-4.13408903637085E-14,-0.92318579281223,0.384353993019006));
#20177=DIRECTION('center_axis',(-1.,0.,0.));
#20178=DIRECTION('ref_axis',(0.,0.,1.));
#20179=DIRECTION('',(-1.,0.,0.));
#20180=DIRECTION('center_axis',(-1.,0.,0.));
#20181=DIRECTION('ref_axis',(0.,0.,1.));
#20182=DIRECTION('center_axis',(-1.,0.,0.));
#20183=DIRECTION('ref_axis',(0.,0.,1.));
#20184=DIRECTION('',(-1.,0.,0.));
#20185=DIRECTION('',(-1.,0.,0.));
#20186=DIRECTION('center_axis',(-1.,0.,0.));
#20187=DIRECTION('ref_axis',(0.,0.,1.));
#20188=DIRECTION('center_axis',(-1.,0.,0.));
#20189=DIRECTION('ref_axis',(0.,0.,1.));
#20190=DIRECTION('',(-1.,0.,0.));
#20191=DIRECTION('center_axis',(-1.,0.,0.));
#20192=DIRECTION('ref_axis',(0.,0.,1.));
#20193=DIRECTION('',(-1.,0.,0.));
#20194=DIRECTION('center_axis',(-1.,0.,0.));
#20195=DIRECTION('ref_axis',(0.,0.,1.));
#20196=DIRECTION('',(-1.,0.,0.));
#20197=DIRECTION('center_axis',(-1.,0.,0.));
#20198=DIRECTION('ref_axis',(0.,0.,1.));
#20199=DIRECTION('',(-1.,0.,0.));
#20200=DIRECTION('center_axis',(-1.,0.,0.));
#20201=DIRECTION('ref_axis',(0.,0.,1.));
#20202=DIRECTION('',(-1.,0.,0.));
#20203=DIRECTION('center_axis',(-1.,0.,0.));
#20204=DIRECTION('ref_axis',(0.,0.,1.));
#20205=DIRECTION('',(-1.,0.,0.));
#20206=DIRECTION('center_axis',(-1.,0.,0.));
#20207=DIRECTION('ref_axis',(0.,0.,1.));
#20208=DIRECTION('',(-1.,0.,0.));
#20209=DIRECTION('center_axis',(-1.,0.,0.));
#20210=DIRECTION('ref_axis',(0.,0.,1.));
#20211=DIRECTION('',(-1.,0.,0.));
#20212=DIRECTION('center_axis',(-1.,0.,0.));
#20213=DIRECTION('ref_axis',(0.,0.,1.));
#20214=DIRECTION('',(-1.,0.,0.));
#20215=DIRECTION('center_axis',(-1.,0.,0.));
#20216=DIRECTION('ref_axis',(0.,0.,1.));
#20217=DIRECTION('',(-1.,0.,0.));
#20218=DIRECTION('center_axis',(-1.,0.,0.));
#20219=DIRECTION('ref_axis',(0.,0.,1.));
#20220=DIRECTION('',(-1.,0.,0.));
#20221=DIRECTION('center_axis',(-1.,0.,0.));
#20222=DIRECTION('ref_axis',(0.,0.,1.));
#20223=DIRECTION('',(-1.,0.,0.));
#20224=DIRECTION('center_axis',(-1.,0.,0.));
#20225=DIRECTION('ref_axis',(0.,0.,1.));
#20226=DIRECTION('',(-1.,0.,0.));
#20227=DIRECTION('center_axis',(-1.,0.,0.));
#20228=DIRECTION('ref_axis',(0.,0.,1.));
#20229=DIRECTION('',(-1.,0.,0.));
#20230=DIRECTION('center_axis',(-1.,0.,0.));
#20231=DIRECTION('ref_axis',(0.,0.,1.));
#20232=DIRECTION('',(-1.,0.,0.));
#20233=DIRECTION('center_axis',(-1.,0.,0.));
#20234=DIRECTION('ref_axis',(0.,0.,1.));
#20235=DIRECTION('',(-1.,0.,0.));
#20236=DIRECTION('center_axis',(-1.,0.,0.));
#20237=DIRECTION('ref_axis',(0.,0.,1.));
#20238=DIRECTION('',(-1.,0.,0.));
#20239=DIRECTION('center_axis',(-1.,0.,0.));
#20240=DIRECTION('ref_axis',(0.,0.,1.));
#20241=DIRECTION('',(-1.,0.,0.));
#20242=DIRECTION('center_axis',(-1.,0.,0.));
#20243=DIRECTION('ref_axis',(0.,0.,1.));
#20244=DIRECTION('',(-1.,0.,0.));
#20245=DIRECTION('center_axis',(-1.,0.,0.));
#20246=DIRECTION('ref_axis',(0.,0.,1.));
#20247=DIRECTION('',(-1.,0.,0.));
#20248=DIRECTION('center_axis',(-1.,0.,0.));
#20249=DIRECTION('ref_axis',(0.,0.,1.));
#20250=DIRECTION('',(-1.,0.,0.));
#20251=DIRECTION('center_axis',(-1.,0.,0.));
#20252=DIRECTION('ref_axis',(0.,0.,1.));
#20253=DIRECTION('',(-1.,0.,0.));
#20254=DIRECTION('center_axis',(-1.,0.,0.));
#20255=DIRECTION('ref_axis',(0.,0.,1.));
#20256=DIRECTION('',(-1.,0.,0.));
#20257=DIRECTION('center_axis',(1.,0.,0.));
#20258=DIRECTION('ref_axis',(0.,0.,-1.));
#20259=DIRECTION('center_axis',(-1.,0.,0.));
#20260=DIRECTION('ref_axis',(0.,0.,1.));
#20261=DIRECTION('',(-0.707106781186486,-8.65956056235569E-17,-0.707106781186609));
#20262=DIRECTION('center_axis',(-1.,0.,0.));
#20263=DIRECTION('ref_axis',(0.,0.,1.));
#20264=DIRECTION('center_axis',(1.,0.,0.));
#20265=DIRECTION('ref_axis',(0.,0.,-1.));
#20266=DIRECTION('center_axis',(1.,0.,0.));
#20267=DIRECTION('ref_axis',(0.,0.,-1.));
#20268=DIRECTION('',(1.,0.,0.));
#20269=DIRECTION('center_axis',(-1.,0.,0.));
#20270=DIRECTION('ref_axis',(0.,0.,1.));
#20271=DIRECTION('center_axis',(1.,0.,0.));
#20272=DIRECTION('ref_axis',(0.,0.,1.));
#20273=DIRECTION('',(1.,0.,0.));
#20274=DIRECTION('center_axis',(1.,0.,0.));
#20275=DIRECTION('ref_axis',(0.,0.,-1.));
#20276=DIRECTION('center_axis',(1.,0.,0.));
#20277=DIRECTION('ref_axis',(0.,0.,1.));
#20278=DIRECTION('center_axis',(-1.,0.,0.));
#20279=DIRECTION('ref_axis',(0.,0.,1.));
#20280=DIRECTION('center_axis',(1.,0.,0.));
#20281=DIRECTION('ref_axis',(0.,0.,-1.));
#20282=DIRECTION('center_axis',(1.,0.,0.));
#20283=DIRECTION('ref_axis',(0.,0.,-1.));
#20284=DIRECTION('center_axis',(0.,-1.,-1.22464679914735E-16));
#20285=DIRECTION('ref_axis',(0.,-1.22464679914735E-16,1.));
#20286=DIRECTION('center_axis',(1.,0.,0.));
#20287=DIRECTION('ref_axis',(0.,0.,-1.));
#20288=DIRECTION('center_axis',(1.,0.,0.));
#20289=DIRECTION('ref_axis',(0.,0.,-1.));
#20290=DIRECTION('center_axis',(1.,0.,0.));
#20291=DIRECTION('ref_axis',(0.,0.,-1.));
#20292=DIRECTION('',(-1.,0.,0.));
#20293=DIRECTION('center_axis',(1.,0.,0.));
#20294=DIRECTION('ref_axis',(0.,-0.308832433911277,0.951116463827873));
#20295=DIRECTION('center_axis',(1.,0.,0.));
#20296=DIRECTION('ref_axis',(0.,-0.308832433911277,0.951116463827873));
#20297=DIRECTION('',(-1.,0.,0.));
#20298=DIRECTION('center_axis',(1.,0.,0.));
#20299=DIRECTION('ref_axis',(0.,-0.308832433911277,0.951116463827873));
#20300=DIRECTION('center_axis',(1.,0.,0.));
#20301=DIRECTION('ref_axis',(0.,-0.308832433911277,0.951116463827873));
#20302=DIRECTION('center_axis',(1.,0.,0.));
#20303=DIRECTION('ref_axis',(0.,0.,-1.));
#20304=DIRECTION('center_axis',(1.,0.,0.));
#20305=DIRECTION('ref_axis',(0.,0.,-1.));
#20306=DIRECTION('center_axis',(0.,-1.,-1.22464679914735E-16));
#20307=DIRECTION('ref_axis',(0.,-1.22464679914735E-16,1.));
#20308=DIRECTION('center_axis',(1.,0.,0.));
#20309=DIRECTION('ref_axis',(0.,0.,-1.));
#20310=DIRECTION('center_axis',(1.,0.,0.));
#20311=DIRECTION('ref_axis',(0.,0.,-1.));
#20312=DIRECTION('center_axis',(1.,0.,0.));
#20313=DIRECTION('ref_axis',(0.,0.,-1.));
#20314=DIRECTION('',(-1.,0.,0.));
#20315=DIRECTION('center_axis',(1.,0.,0.));
#20316=DIRECTION('ref_axis',(0.,0.,-1.));
#20317=DIRECTION('center_axis',(1.,0.,0.));
#20318=DIRECTION('ref_axis',(0.,0.,-1.));
#20319=DIRECTION('',(1.,0.,0.));
#20320=DIRECTION('center_axis',(1.,0.,0.));
#20321=DIRECTION('ref_axis',(0.,0.,-1.));
#20322=DIRECTION('center_axis',(-1.,0.,0.));
#20323=DIRECTION('ref_axis',(0.,0.,1.));
#20324=DIRECTION('center_axis',(1.,0.,0.));
#20325=DIRECTION('ref_axis',(0.,0.,-1.));
#20326=DIRECTION('center_axis',(1.,0.,0.));
#20327=DIRECTION('ref_axis',(0.,0.,-1.));
#20328=DIRECTION('center_axis',(1.,0.,0.));
#20329=DIRECTION('ref_axis',(0.,0.,-1.));
#20330=DIRECTION('center_axis',(-1.,0.,0.));
#20331=DIRECTION('ref_axis',(0.,0.,1.));
#20332=DIRECTION('center_axis',(-1.,0.,0.));
#20333=DIRECTION('ref_axis',(0.,0.,1.));
#20334=DIRECTION('',(-3.94745964311166E-15,0.774569892332855,0.632488325498163));
#20335=DIRECTION('',(-9.86864910777916E-16,0.774569892332855,0.632488325498162));
#20336=DIRECTION('center_axis',(-1.,0.,0.));
#20337=DIRECTION('ref_axis',(0.,0.,1.));
#20338=DIRECTION('',(0.,-0.308832433911277,0.951116463827873));
#20339=DIRECTION('',(0.,-0.308832433911277,0.951116463827873));
#20340=DIRECTION('center_axis',(-1.,0.,0.));
#20341=DIRECTION('ref_axis',(0.,0.,1.));
#20342=DIRECTION('center_axis',(-7.62720960372908E-16,-0.999390827019096,
-0.0348994967025015));
#20343=DIRECTION('ref_axis',(3.27874698101124E-34,0.0348994967025015,-0.999390827019096));
#20344=DIRECTION('',(0.499999999999987,0.0302238507236574,-0.865497844507684));
#20345=DIRECTION('',(0.499999999999985,-0.0302238507236573,0.865497844507685));
#20346=DIRECTION('center_axis',(1.,4.0668225646129E-15,-2.78321068817773E-14));
#20347=DIRECTION('ref_axis',(-2.89386232545955E-14,0.0348994967025012,-0.999390827019096));
#20348=DIRECTION('axis',(0.,0.,1.));
#20349=DIRECTION('refdir',(1.,0.,0.));
#20350=DIRECTION('center_axis',(0.,-1.,0.));
#20351=DIRECTION('ref_axis',(0.,0.,-1.));
#20352=DIRECTION('center_axis',(0.,1.,0.));
#20353=DIRECTION('ref_axis',(0.,0.,1.));
#20354=DIRECTION('',(0.,-1.,0.));
#20355=DIRECTION('center_axis',(0.,-1.,0.));
#20356=DIRECTION('ref_axis',(0.,0.,1.));
#20357=DIRECTION('center_axis',(0.,-1.,0.));
#20358=DIRECTION('ref_axis',(0.,0.,-1.));
#20359=DIRECTION('center_axis',(0.,1.,0.));
#20360=DIRECTION('ref_axis',(0.,0.,1.));
#20361=DIRECTION('',(0.,1.,0.));
#20362=DIRECTION('center_axis',(0.,1.,0.));
#20363=DIRECTION('ref_axis',(0.,0.,1.));
#20364=DIRECTION('center_axis',(0.,1.,0.));
#20365=DIRECTION('ref_axis',(0.,0.,1.));
#20366=DIRECTION('center_axis',(0.,1.,0.));
#20367=DIRECTION('ref_axis',(0.,0.,1.));
#20368=DIRECTION('center_axis',(0.,1.,0.));
#20369=DIRECTION('ref_axis',(0.,0.,1.));
#20370=DIRECTION('axis',(0.,0.,1.));
#20371=DIRECTION('refdir',(1.,0.,0.));
#20372=DIRECTION('center_axis',(0.,-1.,0.));
#20373=DIRECTION('ref_axis',(0.,0.,-1.));
#20374=DIRECTION('center_axis',(0.,1.,0.));
#20375=DIRECTION('ref_axis',(0.,0.,1.));
#20376=DIRECTION('',(0.,-1.,0.));
#20377=DIRECTION('center_axis',(0.,1.,0.));
#20378=DIRECTION('ref_axis',(0.,0.,1.));
#20379=DIRECTION('center_axis',(0.,-1.,0.));
#20380=DIRECTION('ref_axis',(0.,0.,-1.));
#20381=DIRECTION('center_axis',(0.,1.,0.));
#20382=DIRECTION('ref_axis',(0.,0.,1.));
#20383=DIRECTION('',(0.,1.,0.));
#20384=DIRECTION('center_axis',(0.,1.,0.));
#20385=DIRECTION('ref_axis',(0.,0.,1.));
#20386=DIRECTION('center_axis',(0.,1.,0.));
#20387=DIRECTION('ref_axis',(0.,0.,1.));
#20388=DIRECTION('center_axis',(0.,1.,0.));
#20389=DIRECTION('ref_axis',(0.,0.,1.));
#20390=DIRECTION('axis',(0.,0.,1.));
#20391=DIRECTION('refdir',(1.,0.,0.));
#20392=DIRECTION('center_axis',(0.,0.,-1.));
#20393=DIRECTION('ref_axis',(-1.,0.,0.));
#20394=DIRECTION('center_axis',(0.,0.,-1.));
#20395=DIRECTION('ref_axis',(-1.,0.,0.));
#20396=DIRECTION('center_axis',(0.,0.,-1.));
#20397=DIRECTION('ref_axis',(-1.,0.,0.));
#20398=DIRECTION('center_axis',(-1.22464679914735E-16,-1.,0.));
#20399=DIRECTION('ref_axis',(1.,-1.22464679914735E-16,0.));
#20400=DIRECTION('center_axis',(0.,0.,1.));
#20401=DIRECTION('ref_axis',(-1.,0.,0.));
#20402=DIRECTION('center_axis',(0.,0.,1.));
#20403=DIRECTION('ref_axis',(1.,0.,0.));
#20404=DIRECTION('center_axis',(0.,0.,1.));
#20405=DIRECTION('ref_axis',(1.,0.,0.));
#20406=DIRECTION('center_axis',(1.22464679914735E-16,-1.,0.));
#20407=DIRECTION('ref_axis',(-1.,-1.22464679914735E-16,0.));
#20408=DIRECTION('center_axis',(0.,0.,1.));
#20409=DIRECTION('ref_axis',(1.,0.,0.));
#20410=DIRECTION('center_axis',(0.,0.,1.));
#20411=DIRECTION('ref_axis',(1.,0.,0.));
#20412=DIRECTION('',(0.,0.,-1.));
#20413=DIRECTION('center_axis',(0.,0.,1.));
#20414=DIRECTION('ref_axis',(1.,0.,0.));
#20415=DIRECTION('center_axis',(0.,0.,1.));
#20416=DIRECTION('ref_axis',(1.,0.,0.));
#20417=DIRECTION('',(0.,0.,-1.));
#20418=DIRECTION('center_axis',(0.,0.,-1.));
#20419=DIRECTION('ref_axis',(-1.,0.,0.));
#20420=DIRECTION('center_axis',(0.,0.,1.));
#20421=DIRECTION('ref_axis',(1.,0.,0.));
#20422=DIRECTION('axis',(0.,0.,1.));
#20423=DIRECTION('refdir',(1.,0.,0.));
#20424=DIRECTION('center_axis',(0.,0.,-1.));
#20425=DIRECTION('ref_axis',(-1.,0.,0.));
#20426=DIRECTION('center_axis',(0.,0.,-1.));
#20427=DIRECTION('ref_axis',(-1.,0.,0.));
#20428=DIRECTION('center_axis',(-1.22464679914735E-16,-1.,0.));
#20429=DIRECTION('ref_axis',(1.,-1.22464679914735E-16,0.));
#20430=DIRECTION('center_axis',(0.,0.,-1.));
#20431=DIRECTION('ref_axis',(-1.,0.,0.));
#20432=DIRECTION('center_axis',(0.,0.,-1.));
#20433=DIRECTION('ref_axis',(-1.,0.,0.));
#20434=DIRECTION('',(0.,0.,1.));
#20435=DIRECTION('center_axis',(0.,0.,-1.));
#20436=DIRECTION('ref_axis',(-1.,0.,0.));
#20437=DIRECTION('center_axis',(0.,0.,-1.));
#20438=DIRECTION('ref_axis',(-1.,0.,0.));
#20439=DIRECTION('',(-0.707106781186547,8.65956056235493E-17,0.707106781186548));
#20440=DIRECTION('center_axis',(0.,0.,-1.));
#20441=DIRECTION('ref_axis',(-1.,0.,0.));
#20442=DIRECTION('center_axis',(0.,0.,-1.));
#20443=DIRECTION('ref_axis',(-1.,0.,0.));
#20444=DIRECTION('center_axis',(0.,0.,-1.));
#20445=DIRECTION('ref_axis',(-1.,0.,0.));
#20446=DIRECTION('',(0.,0.,1.));
#20447=DIRECTION('center_axis',(0.,0.,-1.));
#20448=DIRECTION('ref_axis',(-1.,0.,0.));
#20449=DIRECTION('center_axis',(0.,0.,-1.));
#20450=DIRECTION('ref_axis',(-1.,0.,0.));
#20451=DIRECTION('',(-0.707106781186549,8.65956056235495E-17,0.707106781186547));
#20452=DIRECTION('center_axis',(0.,0.,-1.));
#20453=DIRECTION('ref_axis',(-1.,0.,0.));
#20454=DIRECTION('center_axis',(1.,6.12323399573677E-17,0.));
#20455=DIRECTION('ref_axis',(0.,1.,0.));
#20456=DIRECTION('center_axis',(0.,1.22464679914735E-16,-1.));
#20457=DIRECTION('ref_axis',(0.,-1.,-1.22464679914735E-16));
#20458=DIRECTION('center_axis',(0.,0.,-1.));
#20459=DIRECTION('ref_axis',(-1.,0.,0.));
#20460=DIRECTION('center_axis',(0.,0.,-1.));
#20461=DIRECTION('ref_axis',(-1.,0.,0.));
#20462=DIRECTION('',(0.,0.,1.));
#20463=DIRECTION('center_axis',(0.,0.,-1.));
#20464=DIRECTION('ref_axis',(-1.,0.,0.));
#20465=DIRECTION('center_axis',(0.,0.,-1.));
#20466=DIRECTION('ref_axis',(-1.,0.,0.));
#20467=DIRECTION('center_axis',(0.,0.,1.));
#20468=DIRECTION('ref_axis',(1.,0.,0.));
#20469=DIRECTION('center_axis',(0.,0.,1.));
#20470=DIRECTION('ref_axis',(1.,0.,0.));
#20471=DIRECTION('axis',(0.,0.,1.));
#20472=DIRECTION('refdir',(1.,0.,0.));
#20473=DIRECTION('center_axis',(1.,0.,0.));
#20474=DIRECTION('ref_axis',(0.,0.,-1.));
#20475=DIRECTION('center_axis',(1.,0.,0.));
#20476=DIRECTION('ref_axis',(0.,0.,1.));
#20477=DIRECTION('',(-0.618390361344798,9.62414507819028E-17,-0.785871084209013));
#20478=DIRECTION('center_axis',(-1.,0.,0.));
#20479=DIRECTION('ref_axis',(0.,0.,-1.));
#20480=DIRECTION('center_axis',(0.,0.,1.));
#20481=DIRECTION('ref_axis',(1.,8.88178419700125E-16,0.));
#20482=DIRECTION('center_axis',(0.378876330722911,-1.20404638253675E-15,
0.925447311313801));
#20483=DIRECTION('ref_axis',(0.925447311313801,1.02297272535146E-30,-0.378876330722911));
#20484=DIRECTION('center_axis',(-1.,1.16846812913649E-29,-1.34715203352919E-14));
#20485=DIRECTION('ref_axis',(-1.34715203352919E-14,-4.74710593547472E-45,
1.));
#20486=DIRECTION('center_axis',(0.,-0.515078753637713,0.857142857142857));
#20487=DIRECTION('ref_axis',(0.,-0.857142857142857,-0.515078753637713));
#20488=DIRECTION('center_axis',(-1.,0.,0.));
#20489=DIRECTION('ref_axis',(0.,0.,1.));
#20490=DIRECTION('center_axis',(-1.,0.,0.));
#20491=DIRECTION('ref_axis',(0.,0.,1.));
#20492=DIRECTION('center_axis',(0.,0.515078753637713,0.857142857142857));
#20493=DIRECTION('ref_axis',(0.,0.857142857142857,-0.515078753637713));
#20494=DIRECTION('center_axis',(-1.,0.,0.));
#20495=DIRECTION('ref_axis',(0.,0.,1.));
#20496=DIRECTION('center_axis',(-1.,0.,0.));
#20497=DIRECTION('ref_axis',(0.,0.,1.));
#20498=DIRECTION('',(-1.,0.,0.));
#20499=DIRECTION('center_axis',(-1.,0.,0.));
#20500=DIRECTION('ref_axis',(0.,0.,1.));
#20501=DIRECTION('',(1.,0.,0.));
#20502=DIRECTION('center_axis',(-1.,0.,0.));
#20503=DIRECTION('ref_axis',(0.,0.,1.));
#20504=DIRECTION('center_axis',(-1.,0.,0.));
#20505=DIRECTION('ref_axis',(0.,0.,1.));
#20506=DIRECTION('center_axis',(0.,6.12323399573677E-17,-1.));
#20507=DIRECTION('ref_axis',(0.,1.,0.));
#20508=DIRECTION('center_axis',(1.,0.,0.));
#20509=DIRECTION('ref_axis',(0.,-1.,0.));
#20510=DIRECTION('center_axis',(0.,0.,1.));
#20511=DIRECTION('ref_axis',(-1.,0.,0.));
#20512=DIRECTION('center_axis',(-1.,0.,0.));
#20513=DIRECTION('ref_axis',(0.,0.,1.));
#20514=DIRECTION('center_axis',(0.,0.,1.));
#20515=DIRECTION('ref_axis',(-1.,-1.77635683940025E-15,0.));
#20516=DIRECTION('center_axis',(1.,0.,0.));
#20517=DIRECTION('ref_axis',(0.,0.,-1.));
#20518=DIRECTION('center_axis',(-1.,0.,0.));
#20519=DIRECTION('ref_axis',(0.,0.,1.));
#20520=DIRECTION('',(-0.992962790709924,1.45030946266966E-17,-0.118426754855312));
#20521=DIRECTION('center_axis',(-1.,0.,0.));
#20522=DIRECTION('ref_axis',(0.,0.,1.));
#20523=DIRECTION('center_axis',(-0.129239030503541,0.903475790448336,-0.408691532905026));
#20524=DIRECTION('ref_axis',(0.134650954949434,0.42432007345752,0.895444914884333));
#20525=DIRECTION('center_axis',(1.,-3.74939945665464E-33,6.12323399573677E-17));
#20526=DIRECTION('ref_axis',(0.,-6.12323399573677E-17,1.));
#20527=DIRECTION('center_axis',(0.,1.,0.));
#20528=DIRECTION('ref_axis',(1.87495354061429E-14,0.,-1.));
#20529=DIRECTION('center_axis',(7.01804016390762E-16,-1.,0.));
#20530=DIRECTION('ref_axis',(-1.,-7.01804016390762E-16,1.06581410364015E-14));
#20531=DIRECTION('center_axis',(-1.,0.,0.));
#20532=DIRECTION('ref_axis',(0.,0.,1.));
#20533=DIRECTION('',(1.,0.,0.));
#20534=DIRECTION('',(-1.,0.,0.));
#20535=DIRECTION('center_axis',(-1.,0.,0.));
#20536=DIRECTION('ref_axis',(0.,0.,1.));
#20537=DIRECTION('',(-1.,0.,0.));
#20538=DIRECTION('center_axis',(1.,0.,0.));
#20539=DIRECTION('ref_axis',(0.,0.,-1.));
#20540=DIRECTION('center_axis',(0.,0.,-1.));
#20541=DIRECTION('ref_axis',(-1.,0.,0.));
#20542=DIRECTION('center_axis',(0.,0.,1.));
#20543=DIRECTION('ref_axis',(1.,0.,0.));
#20544=DIRECTION('center_axis',(0.,0.,-1.));
#20545=DIRECTION('ref_axis',(-1.,0.,0.));
#20546=DIRECTION('center_axis',(0.,0.,1.));
#20547=DIRECTION('ref_axis',(1.,0.,0.));
#20548=DIRECTION('center_axis',(0.,0.,1.));
#20549=DIRECTION('ref_axis',(-1.,7.6571373978539E-16,0.));
#20550=DIRECTION('',(0.,0.,1.));
#20551=DIRECTION('',(0.,0.,1.));
#20552=DIRECTION('center_axis',(0.,0.,1.));
#20553=DIRECTION('ref_axis',(1.,0.,0.));
#20554=DIRECTION('center_axis',(0.,0.,-1.));
#20555=DIRECTION('ref_axis',(1.,4.33680868994201E-15,0.));
#20556=DIRECTION('',(0.,0.,1.));
#20557=DIRECTION('center_axis',(0.,0.,1.));
#20558=DIRECTION('ref_axis',(1.,0.,0.));
#20559=DIRECTION('center_axis',(0.,0.,1.));
#20560=DIRECTION('ref_axis',(1.,0.,0.));
#20561=DIRECTION('center_axis',(0.,0.,1.));
#20562=DIRECTION('ref_axis',(1.,0.,0.));
#20563=DIRECTION('',(0.,0.,1.));
#20564=DIRECTION('center_axis',(0.,0.,-1.));
#20565=DIRECTION('ref_axis',(1.,-2.60208521396521E-15,0.));
#20566=DIRECTION('center_axis',(0.,1.,0.));
#20567=DIRECTION('ref_axis',(0.,0.,1.));
#20568=DIRECTION('center_axis',(0.,-1.,0.));
#20569=DIRECTION('ref_axis',(-6.9269116917139E-15,0.,1.));
#20570=DIRECTION('',(-1.,0.,0.));
#20571=DIRECTION('center_axis',(7.01804016390762E-16,-1.,0.));
#20572=DIRECTION('ref_axis',(1.,7.01804016390762E-16,0.));
#20573=DIRECTION('',(1.,7.01804016390762E-16,0.));
#20574=DIRECTION('center_axis',(-7.01804016390762E-16,1.,0.));
#20575=DIRECTION('ref_axis',(1.,7.01804016390762E-16,0.));
#20576=DIRECTION('center_axis',(0.709785481558855,-0.704116397237294,-0.020607506152819));
#20577=DIRECTION('ref_axis',(0.704265953185076,0.709936241633231,4.28924729850355E-17));
#20578=DIRECTION('center_axis',(0.29037131728916,-0.353646401377125,-0.889167431302321));
#20579=DIRECTION('ref_axis',(-7.39118707684208E-18,0.929203026942477,-0.369569661526671));
#20580=DIRECTION('center_axis',(0.348558970379625,-0.482776543868745,-0.803388730850791));
#20581=DIRECTION('ref_axis',(-1.8398092574652E-17,0.857142857142857,-0.515078753637713));
#20582=DIRECTION('center_axis',(1.,0.,0.));
#20583=DIRECTION('ref_axis',(0.,0.515078753637713,0.857142857142857));
#20584=DIRECTION('center_axis',(1.,0.,0.));
#20585=DIRECTION('ref_axis',(0.,0.,-1.));
#20586=DIRECTION('center_axis',(-1.,0.,0.));
#20587=DIRECTION('ref_axis',(0.,0.,1.));
#20588=DIRECTION('center_axis',(1.,6.93889390390723E-15,1.15470174302502E-14));
#20589=DIRECTION('ref_axis',(1.15470174302502E-14,-1.61729683642884E-29,
-1.));
#20590=DIRECTION('center_axis',(0.,0.,1.));
#20591=DIRECTION('ref_axis',(1.,0.,0.));
#20592=DIRECTION('center_axis',(-0.378876330722912,4.01348794178917E-16,
-0.925447311313801));
#20593=DIRECTION('ref_axis',(-0.925447311313801,1.31246556823689E-31,0.378876330722912));
#20594=DIRECTION('center_axis',(0.,1.,0.));
#20595=DIRECTION('ref_axis',(0.,0.,1.));
#20596=DIRECTION('center_axis',(-0.489525396383285,0.,-0.871989040238343));
#20597=DIRECTION('ref_axis',(-0.871989040238343,0.,0.489525396383285));
#20598=DIRECTION('center_axis',(1.,0.,0.));
#20599=DIRECTION('ref_axis',(0.,-1.,0.));
#20600=DIRECTION('center_axis',(-0.585365170384224,0.810768328674619,0.00152791335295939));
#20601=DIRECTION('ref_axis',(-0.810769275053396,-0.585365853658539,-3.50084822314998E-20));
#20602=DIRECTION('center_axis',(0.58536517038422,0.810768328674621,-0.00152791335296999));
#20603=DIRECTION('ref_axis',(-0.810769275053399,0.585365853658535,-2.27653634851535E-20));
#20604=DIRECTION('center_axis',(1.,0.,0.));
#20605=DIRECTION('ref_axis',(0.,-1.,0.));
#20606=DIRECTION('center_axis',(0.489525396383287,0.,0.871989040238343));
#20607=DIRECTION('ref_axis',(0.871989040238342,0.,-0.489525396383287));
#20608=DIRECTION('center_axis',(7.01804016390762E-16,-1.,0.));
#20609=DIRECTION('ref_axis',(1.,7.60106174710418E-16,0.));
#20610=DIRECTION('center_axis',(-1.,0.,0.));
#20611=DIRECTION('ref_axis',(0.,0.,1.));
#20612=DIRECTION('center_axis',(-1.,0.,0.));
#20613=DIRECTION('ref_axis',(0.,0.,1.));
#20614=DIRECTION('center_axis',(1.,0.,0.));
#20615=DIRECTION('ref_axis',(0.,0.515078753637712,-0.857142857142858));
#20616=DIRECTION('center_axis',(-0.348558970379622,-0.482776543868745,0.803388730850793));
#20617=DIRECTION('ref_axis',(2.32069397924157E-17,-0.857142857142857,-0.515078753637712));
#20618=DIRECTION('center_axis',(-0.29037131728916,-0.353646401377124,0.889167431302321));
#20619=DIRECTION('ref_axis',(-4.59831187317044E-17,-0.929203026942477,-0.369569661526671));
#20620=DIRECTION('center_axis',(-0.709785481558847,-0.7041163972373,0.0206075061528517));
#20621=DIRECTION('ref_axis',(0.704265953185083,-0.709936241633223,2.61261679533882E-17));
#20622=DIRECTION('axis',(0.,0.,1.));
#20623=DIRECTION('refdir',(1.,0.,0.));
#20624=DIRECTION('center_axis',(0.,6.12323399573677E-17,-1.));
#20625=DIRECTION('ref_axis',(0.,1.,0.));
#20626=DIRECTION('center_axis',(-1.,1.22464679914735E-16,0.));
#20627=DIRECTION('ref_axis',(-1.22464679914735E-16,-1.,0.));
#20628=DIRECTION('center_axis',(0.,0.,1.));
#20629=DIRECTION('ref_axis',(1.,0.,0.));
#20630=DIRECTION('center_axis',(-1.,0.,0.));
#20631=DIRECTION('ref_axis',(0.,0.,1.));
#20632=DIRECTION('center_axis',(0.,0.,-1.));
#20633=DIRECTION('ref_axis',(-1.,0.,0.));
#20634=DIRECTION('center_axis',(0.,0.,1.));
#20635=DIRECTION('ref_axis',(1.,0.,0.));
#20636=DIRECTION('center_axis',(0.,0.,1.));
#20637=DIRECTION('ref_axis',(1.,0.,0.));
#20638=DIRECTION('',(0.,0.,1.));
#20639=DIRECTION('center_axis',(0.,0.,1.));
#20640=DIRECTION('ref_axis',(1.,0.,0.));
#20641=DIRECTION('center_axis',(0.,6.12323399573677E-17,-1.));
#20642=DIRECTION('ref_axis',(0.,1.,0.));
#20643=DIRECTION('center_axis',(0.,0.,-1.));
#20644=DIRECTION('ref_axis',(-1.,0.,0.));
#20645=DIRECTION('center_axis',(-1.,0.,0.));
#20646=DIRECTION('ref_axis',(0.,0.,1.));
#20647=DIRECTION('center_axis',(0.,0.,1.));
#20648=DIRECTION('ref_axis',(1.,0.,0.));
#20649=DIRECTION('center_axis',(-1.,0.,0.));
#20650=DIRECTION('ref_axis',(0.,0.,1.));
#20651=DIRECTION('',(0.999433833160616,4.1203734923357E-18,0.033645402863948));
#20652=DIRECTION('center_axis',(-1.,0.,0.));
#20653=DIRECTION('ref_axis',(0.,0.,1.));
#20654=DIRECTION('center_axis',(-1.,0.,0.));
#20655=DIRECTION('ref_axis',(0.,0.,1.));
#20656=DIRECTION('',(1.,0.,0.));
#20657=DIRECTION('center_axis',(-1.,0.,0.));
#20658=DIRECTION('ref_axis',(0.,0.,1.));
#20659=DIRECTION('center_axis',(-1.,0.,0.));
#20660=DIRECTION('ref_axis',(0.,0.,1.));
#20661=DIRECTION('',(0.707106781186548,8.65956056235493E-17,0.707106781186547));
#20662=DIRECTION('center_axis',(-1.,0.,0.));
#20663=DIRECTION('ref_axis',(0.,0.,1.));
#20664=DIRECTION('center_axis',(-1.,0.,0.));
#20665=DIRECTION('ref_axis',(0.,0.,1.));
#20666=DIRECTION('center_axis',(0.,0.,-1.));
#20667=DIRECTION('ref_axis',(-1.,0.,0.));
#20668=DIRECTION('center_axis',(0.,0.,1.));
#20669=DIRECTION('ref_axis',(1.,0.,0.));
#20670=DIRECTION('axis',(0.,0.,1.));
#20671=DIRECTION('refdir',(1.,0.,0.));
#20672=DIRECTION('center_axis',(0.,1.,0.));
#20673=DIRECTION('ref_axis',(0.,0.,1.));
#20674=DIRECTION('center_axis',(0.,-1.,0.));
#20675=DIRECTION('ref_axis',(0.,0.,1.));
#20676=DIRECTION('center_axis',(0.,1.,0.));
#20677=DIRECTION('ref_axis',(0.,0.,1.));
#20678=DIRECTION('center_axis',(0.,1.,0.));
#20679=DIRECTION('ref_axis',(0.,0.,1.));
#20680=DIRECTION('center_axis',(0.,1.,0.));
#20681=DIRECTION('ref_axis',(-1.,0.,-1.83697019872103E-16));
#20682=DIRECTION('center_axis',(0.,-1.,0.));
#20683=DIRECTION('ref_axis',(1.89242561015652E-15,0.,1.));
#20684=DIRECTION('',(0.,1.,0.));
#20685=DIRECTION('center_axis',(0.,1.,0.));
#20686=DIRECTION('ref_axis',(0.,0.,1.));
#20687=DIRECTION('center_axis',(0.,1.,0.));
#20688=DIRECTION('ref_axis',(0.,0.,1.));
#20689=DIRECTION('',(0.,1.,0.));
#20690=DIRECTION('center_axis',(1.,0.,0.));
#20691=DIRECTION('ref_axis',(0.,0.,-1.));
#20692=DIRECTION('center_axis',(1.,0.,0.));
#20693=DIRECTION('ref_axis',(0.,0.,1.));
#20694=DIRECTION('',(-0.672379811723126,9.06491294391023E-17,-0.740206315014384));
#20695=DIRECTION('center_axis',(-1.,0.,0.));
#20696=DIRECTION('ref_axis',(0.,0.,-1.));
#20697=DIRECTION('center_axis',(-1.,0.,0.));
#20698=DIRECTION('ref_axis',(0.,1.,6.12323399573677E-17));
#20699=DIRECTION('center_axis',(0.,1.,0.));
#20700=DIRECTION('ref_axis',(0.,0.,1.));
#20701=DIRECTION('center_axis',(-1.,0.,0.));
#20702=DIRECTION('ref_axis',(0.,0.,1.));
#20703=DIRECTION('center_axis',(0.,1.,0.));
#20704=DIRECTION('ref_axis',(0.,0.,1.));
#20705=DIRECTION('center_axis',(-1.,0.,0.));
#20706=DIRECTION('ref_axis',(0.,0.,1.));
#20707=DIRECTION('center_axis',(1.,6.12323399573677E-17,-7.49879891330929E-33));
#20708=DIRECTION('ref_axis',(0.,1.,-1.22464679914735E-16));
#20709=DIRECTION('center_axis',(0.,-1.,0.));
#20710=DIRECTION('ref_axis',(0.,0.,1.));
#20711=DIRECTION('center_axis',(-1.,0.,0.));
#20712=DIRECTION('ref_axis',(0.,0.,1.));
#20713=DIRECTION('center_axis',(0.,-1.,0.));
#20714=DIRECTION('ref_axis',(-5.56057725117657E-13,0.,1.));
#20715=DIRECTION('center_axis',(-1.,0.,0.));
#20716=DIRECTION('ref_axis',(0.,0.,1.));
#20717=DIRECTION('',(-1.,0.,0.));
#20718=DIRECTION('center_axis',(-1.,0.,0.));
#20719=DIRECTION('ref_axis',(0.,0.,1.));
#20720=DIRECTION('center_axis',(1.,0.,0.));
#20721=DIRECTION('ref_axis',(0.,0.,-1.));
#20722=DIRECTION('center_axis',(-1.,0.,0.));
#20723=DIRECTION('ref_axis',(0.,0.,1.));
#20724=DIRECTION('',(-0.998849229226133,5.87347712983446E-18,-0.0479605804214227));
#20725=DIRECTION('center_axis',(-1.,0.,0.));
#20726=DIRECTION('ref_axis',(0.,0.,1.));
#20727=DIRECTION('center_axis',(0.,6.12323399573676E-17,-1.));
#20728=DIRECTION('ref_axis',(0.,1.,0.));
#20729=DIRECTION('center_axis',(0.,0.,-1.));
#20730=DIRECTION('ref_axis',(1.,0.,0.));
#20731=DIRECTION('center_axis',(0.,1.,0.));
#20732=DIRECTION('ref_axis',(0.,0.,1.));
#20733=DIRECTION('center_axis',(-1.,0.,0.));
#20734=DIRECTION('ref_axis',(0.,-1.,0.));
#20735=DIRECTION('center_axis',(0.,1.,0.));
#20736=DIRECTION('ref_axis',(0.,0.,1.));
#20737=DIRECTION('center_axis',(-1.,0.,0.));
#20738=DIRECTION('ref_axis',(0.,-1.,0.));
#20739=DIRECTION('center_axis',(0.,0.,1.));
#20740=DIRECTION('ref_axis',(-1.,0.,0.));
#20741=DIRECTION('center_axis',(1.,0.,0.));
#20742=DIRECTION('ref_axis',(0.,0.,-1.));
#20743=DIRECTION('center_axis',(0.,0.,1.));
#20744=DIRECTION('ref_axis',(1.,0.,0.));
#20745=DIRECTION('',(1.,0.,0.));
#20746=DIRECTION('center_axis',(0.,0.,-1.));
#20747=DIRECTION('ref_axis',(1.,8.88178419700125E-16,0.));
#20748=DIRECTION('center_axis',(0.,0.,-1.));
#20749=DIRECTION('ref_axis',(-1.,0.,0.));
#20750=DIRECTION('center_axis',(0.,0.,1.));
#20751=DIRECTION('ref_axis',(-1.,-1.24344978758018E-14,0.));
#20752=DIRECTION('',(-1.,0.,0.));
#20753=DIRECTION('center_axis',(0.,1.,0.));
#20754=DIRECTION('ref_axis',(0.,0.,1.));
#20755=DIRECTION('center_axis',(0.,1.,0.));
#20756=DIRECTION('ref_axis',(0.,0.,1.));
#20757=DIRECTION('center_axis',(0.,1.,0.));
#20758=DIRECTION('ref_axis',(0.,0.,1.));
#20759=DIRECTION('center_axis',(0.,1.,0.));
#20760=DIRECTION('ref_axis',(0.,0.,1.));
#20761=DIRECTION('center_axis',(-0.706501481417622,-0.707711563247843,-1.83312916504447E-15));
#20762=DIRECTION('ref_axis',(0.707711563247843,-0.706501481417622,-1.95764081482192E-30));
#20763=DIRECTION('center_axis',(0.,0.,-1.));
#20764=DIRECTION('ref_axis',(-1.,0.,0.));
#20765=DIRECTION('center_axis',(0.,1.,0.));
#20766=DIRECTION('ref_axis',(0.0232101926599813,0.,-0.999730607192101));
#20767=DIRECTION('center_axis',(0.,0.,1.));
#20768=DIRECTION('ref_axis',(1.,0.,0.));
#20769=DIRECTION('center_axis',(0.706501481417621,0.707711563247844,0.));
#20770=DIRECTION('ref_axis',(-0.707711563247844,0.706501481417621,0.));
#20771=DIRECTION('axis',(0.,0.,1.));
#20772=DIRECTION('refdir',(1.,0.,0.));
#20773=DIRECTION('center_axis',(0.,6.12323399573677E-17,-1.));
#20774=DIRECTION('ref_axis',(0.,1.,0.));
#20775=DIRECTION('center_axis',(-1.,1.22464679914735E-16,0.));
#20776=DIRECTION('ref_axis',(-1.22464679914735E-16,-1.,0.));
#20777=DIRECTION('center_axis',(0.,0.,1.));
#20778=DIRECTION('ref_axis',(1.,0.,0.));
#20779=DIRECTION('center_axis',(-1.,0.,0.));
#20780=DIRECTION('ref_axis',(0.,0.,1.));
#20781=DIRECTION('center_axis',(0.,0.,-1.));
#20782=DIRECTION('ref_axis',(-1.,0.,0.));
#20783=DIRECTION('center_axis',(0.,0.,1.));
#20784=DIRECTION('ref_axis',(1.,0.,0.));
#20785=DIRECTION('center_axis',(0.,0.,1.));
#20786=DIRECTION('ref_axis',(1.,0.,0.));
#20787=DIRECTION('',(0.,0.,1.));
#20788=DIRECTION('center_axis',(0.,0.,1.));
#20789=DIRECTION('ref_axis',(1.,0.,0.));
#20790=DIRECTION('center_axis',(0.,6.12323399573677E-17,-1.));
#20791=DIRECTION('ref_axis',(0.,1.,0.));
#20792=DIRECTION('center_axis',(0.,0.,-1.));
#20793=DIRECTION('ref_axis',(-1.,0.,0.));
#20794=DIRECTION('center_axis',(-1.,0.,0.));
#20795=DIRECTION('ref_axis',(0.,0.,1.));
#20796=DIRECTION('center_axis',(0.,0.,1.));
#20797=DIRECTION('ref_axis',(1.,0.,0.));
#20798=DIRECTION('center_axis',(-1.,0.,0.));
#20799=DIRECTION('ref_axis',(0.,0.,1.));
#20800=DIRECTION('',(0.99891706524393,5.69782866448938E-18,0.0465263018566368));
#20801=DIRECTION('center_axis',(-1.,0.,0.));
#20802=DIRECTION('ref_axis',(0.,0.,1.));
#20803=DIRECTION('center_axis',(-1.,0.,0.));
#20804=DIRECTION('ref_axis',(0.,0.,1.));
#20805=DIRECTION('',(1.,0.,0.));
#20806=DIRECTION('center_axis',(-1.,0.,0.));
#20807=DIRECTION('ref_axis',(0.,0.,1.));
#20808=DIRECTION('center_axis',(-1.,0.,0.));
#20809=DIRECTION('ref_axis',(0.,0.,1.));
#20810=DIRECTION('',(0.707106781186548,8.65956056235493E-17,0.707106781186547));
#20811=DIRECTION('center_axis',(-1.,0.,0.));
#20812=DIRECTION('ref_axis',(0.,0.,1.));
#20813=DIRECTION('center_axis',(-1.,0.,0.));
#20814=DIRECTION('ref_axis',(0.,0.,1.));
#20815=DIRECTION('center_axis',(0.,0.,-1.));
#20816=DIRECTION('ref_axis',(-1.,0.,0.));
#20817=DIRECTION('center_axis',(0.,0.,1.));
#20818=DIRECTION('ref_axis',(1.,0.,0.));
#20819=DIRECTION('axis',(0.,0.,1.));
#20820=DIRECTION('refdir',(1.,0.,0.));
#20821=DIRECTION('center_axis',(1.,0.,0.));
#20822=DIRECTION('ref_axis',(0.,0.,-1.));
#20823=DIRECTION('center_axis',(1.,0.,0.));
#20824=DIRECTION('ref_axis',(0.,0.,-1.));
#20825=DIRECTION('center_axis',(1.,0.,0.));
#20826=DIRECTION('ref_axis',(0.,0.,-1.));
#20827=DIRECTION('center_axis',(0.,-1.,-1.22464679914735E-16));
#20828=DIRECTION('ref_axis',(0.,-1.22464679914735E-16,1.));
#20829=DIRECTION('center_axis',(-1.,0.,0.));
#20830=DIRECTION('ref_axis',(0.,0.,-1.));
#20831=DIRECTION('center_axis',(-1.,0.,0.));
#20832=DIRECTION('ref_axis',(0.,0.,1.));
#20833=DIRECTION('center_axis',(-1.,0.,0.));
#20834=DIRECTION('ref_axis',(0.,0.,1.));
#20835=DIRECTION('',(0.8,7.34788079488411E-17,0.6));
#20836=DIRECTION('center_axis',(-1.,0.,0.));
#20837=DIRECTION('ref_axis',(0.,0.,1.));
#20838=DIRECTION('center_axis',(-1.,0.,0.));
#20839=DIRECTION('ref_axis',(0.,0.,1.));
#20840=DIRECTION('center_axis',(-1.,0.,0.));
#20841=DIRECTION('ref_axis',(0.,0.,1.));
#20842=DIRECTION('center_axis',(-1.,0.,0.));
#20843=DIRECTION('ref_axis',(0.,0.,1.));
#20844=DIRECTION('',(1.,0.,0.));
#20845=DIRECTION('center_axis',(1.,0.,0.));
#20846=DIRECTION('ref_axis',(0.,0.,-1.));
#20847=DIRECTION('',(-0.600000000000001,9.79717439317882E-17,-0.8));
#20848=DIRECTION('center_axis',(-1.,0.,0.));
#20849=DIRECTION('ref_axis',(0.,0.,1.));
#20850=DIRECTION('center_axis',(-1.,0.,0.));
#20851=DIRECTION('ref_axis',(0.,0.,1.));
#20852=DIRECTION('center_axis',(-1.,0.,0.));
#20853=DIRECTION('ref_axis',(0.,0.,1.));
#20854=DIRECTION('center_axis',(-1.,0.,0.));
#20855=DIRECTION('ref_axis',(0.,0.,1.));
#20856=DIRECTION('',(1.,0.,0.));
#20857=DIRECTION('center_axis',(-1.,0.,0.));
#20858=DIRECTION('ref_axis',(0.,0.,1.));
#20859=DIRECTION('center_axis',(-1.,0.,0.));
#20860=DIRECTION('ref_axis',(0.,0.,1.));
#20861=DIRECTION('',(1.,0.,0.));
#20862=DIRECTION('center_axis',(-1.,0.,0.));
#20863=DIRECTION('ref_axis',(0.,0.,1.));
#20864=DIRECTION('center_axis',(-1.,0.,0.));
#20865=DIRECTION('ref_axis',(0.,0.,1.));
#20866=DIRECTION('',(1.,0.,0.));
#20867=DIRECTION('center_axis',(-1.,0.,0.));
#20868=DIRECTION('ref_axis',(0.,0.,1.));
#20869=DIRECTION('center_axis',(1.,0.,0.));
#20870=DIRECTION('ref_axis',(0.,0.,-1.));
#20871=DIRECTION('center_axis',(-1.,0.,0.));
#20872=DIRECTION('ref_axis',(0.,0.,1.));
#20873=DIRECTION('center_axis',(-1.,0.,0.));
#20874=DIRECTION('ref_axis',(0.,0.,1.));
#20875=DIRECTION('center_axis',(-1.,0.,0.));
#20876=DIRECTION('ref_axis',(0.,0.,1.));
#20877=DIRECTION('axis',(0.,0.,1.));
#20878=DIRECTION('refdir',(1.,0.,0.));
#20879=DIRECTION('center_axis',(-1.,-1.22464679914735E-16,0.));
#20880=DIRECTION('ref_axis',(1.77635683940021E-16,-1.,0.));
#20881=DIRECTION('center_axis',(1.,1.22464679914735E-16,0.));
#20882=DIRECTION('ref_axis',(1.22464679914735E-16,-1.,0.));
#20883=DIRECTION('center_axis',(0.,0.80466773100941,-0.593725393319309));
#20884=DIRECTION('ref_axis',(0.,0.593725393319309,0.80466773100941));
#20885=DIRECTION('center_axis',(-1.,-1.22464679914735E-16,0.));
#20886=DIRECTION('ref_axis',(1.22464679914735E-16,-1.,0.));
#20887=DIRECTION('center_axis',(-1.72383876846542E-15,0.111847407981753,
-0.993725393319383));
#20888=DIRECTION('ref_axis',(1.05814669609279E-32,0.993725393319383,0.111847407981753));
#20889=DIRECTION('center_axis',(1.,1.22464679914735E-16,0.));
#20890=DIRECTION('ref_axis',(-1.22464679914735E-16,1.,0.));
#20891=DIRECTION('center_axis',(-1.,-1.99493199737333E-16,-8.70659703262162E-17));
#20892=DIRECTION('ref_axis',(1.99493199737333E-16,-1.,-1.51035382683587E-33));
#20893=DIRECTION('',(-1.,-1.22464679914735E-16,0.));
#20894=DIRECTION('center_axis',(-1.,0.,0.));
#20895=DIRECTION('ref_axis',(0.,0.,1.));
#20896=DIRECTION('',(1.,1.22464679914735E-16,0.));
#20897=DIRECTION('center_axis',(-1.,-1.22464679914735E-16,0.));
#20898=DIRECTION('ref_axis',(1.77635683940025E-16,-1.,0.));
#20899=DIRECTION('center_axis',(1.,1.22464679914735E-16,0.));
#20900=DIRECTION('ref_axis',(1.22464679914735E-16,-1.,0.));
#20901=DIRECTION('center_axis',(0.,0.916515138991168,0.400000000000001));
#20902=DIRECTION('ref_axis',(0.,-0.400000000000001,0.916515138991168));
#20903=DIRECTION('center_axis',(-1.,-1.22464679914735E-16,0.));
#20904=DIRECTION('ref_axis',(1.22464679914735E-16,-1.,0.));
#20905=DIRECTION('center_axis',(-1.7347234759768E-16,0.916515138991168,
-0.399999999999999));
#20906=DIRECTION('ref_axis',(-1.38807035205952E-32,0.399999999999999,0.916515138991168));
#20907=DIRECTION('center_axis',(1.,1.22464679914735E-16,0.));
#20908=DIRECTION('ref_axis',(-1.33226762955006E-16,1.,0.));
#20909=DIRECTION('center_axis',(-1.,-1.22464679914735E-16,0.));
#20910=DIRECTION('ref_axis',(-1.22464679914735E-16,1.,0.));
#20911=DIRECTION('center_axis',(5.1497468903733E-16,0.804667731009371,0.593725393319361));
#20912=DIRECTION('ref_axis',(-8.01741870322078E-32,-0.593725393319361,0.804667731009371));
#20913=DIRECTION('center_axis',(1.,1.22464679914735E-16,0.));
#20914=DIRECTION('ref_axis',(-1.22464679914735E-16,1.,0.));
#20915=DIRECTION('center_axis',(0.,0.111847407981704,0.993725393319389));
#20916=DIRECTION('ref_axis',(0.,-0.993725393319389,0.111847407981704));
#20917=DIRECTION('center_axis',(-1.,-1.22464679914735E-16,0.));
#20918=DIRECTION('ref_axis',(1.22464679914735E-16,-1.,0.));
#20919=DIRECTION('center_axis',(-1.,0.,0.));
#20920=DIRECTION('ref_axis',(0.,0.,1.));
#20921=DIRECTION('',(1.,1.22464679914735E-16,0.));
#20922=DIRECTION('center_axis',(1.,1.99493199737338E-16,-8.70659703262009E-17));
#20923=DIRECTION('ref_axis',(-1.99493199737338E-16,1.,-1.51035382683516E-33));
#20924=DIRECTION('',(-1.,-1.22464679914735E-16,0.));
#20925=DIRECTION('center_axis',(1.,1.22464679914735E-16,0.));
#20926=DIRECTION('ref_axis',(-1.33226762954999E-16,1.,0.));
#20927=DIRECTION('center_axis',(-1.,-1.22464679914735E-16,0.));
#20928=DIRECTION('ref_axis',(-1.22464679914735E-16,1.,0.));
#20929=DIRECTION('center_axis',(0.,-0.916515138991197,0.399999999999934));
#20930=DIRECTION('ref_axis',(0.,-0.399999999999934,-0.916515138991197));
#20931=DIRECTION('center_axis',(1.,1.22464679914735E-16,0.));
#20932=DIRECTION('ref_axis',(-1.22464679914735E-16,1.,0.));
#20933=DIRECTION('center_axis',(-1.76337267529379E-15,0.916515138991152,
0.400000000000037));
#20934=DIRECTION('ref_axis',(-2.36429138143015E-32,-0.400000000000037,0.916515138991152));
#20935=DIRECTION('center_axis',(-1.,-1.22464679914735E-16,0.));
#20936=DIRECTION('ref_axis',(1.22464679914735E-16,-1.,0.));
#20937=DIRECTION('center_axis',(-1.,0.,0.));
#20938=DIRECTION('ref_axis',(0.,0.,1.));
#20939=DIRECTION('',(1.,1.22464679914735E-16,0.));
#20940=DIRECTION('center_axis',(1.,2.13362867122434E-16,4.30616635022195E-17));
#20941=DIRECTION('ref_axis',(-2.13362867122434E-16,1.,1.49749836094217E-34));
#20942=DIRECTION('',(-1.,-1.22464679914735E-16,0.));
#20943=DIRECTION('center_axis',(1.,1.22464679914735E-16,0.));
#20944=DIRECTION('ref_axis',(-1.33226762955E-16,1.,0.));
#20945=DIRECTION('center_axis',(-1.,-1.22464679914735E-16,0.));
#20946=DIRECTION('ref_axis',(-1.22464679914735E-16,1.,0.));
#20947=DIRECTION('center_axis',(0.,-0.111847407981938,0.993725393319363));
#20948=DIRECTION('ref_axis',(0.,-0.993725393319363,-0.111847407981938));
#20949=DIRECTION('center_axis',(1.,1.22464679914735E-16,0.));
#20950=DIRECTION('ref_axis',(-1.22464679914735E-16,1.,0.));
#20951=DIRECTION('center_axis',(0.,0.804667731009333,-0.593725393319413));
#20952=DIRECTION('ref_axis',(0.,0.593725393319413,0.804667731009333));
#20953=DIRECTION('center_axis',(-1.,-1.22464679914735E-16,0.));
#20954=DIRECTION('ref_axis',(1.77635683940011E-16,-1.,0.));
#20955=DIRECTION('center_axis',(1.,1.22464679914735E-16,0.));
#20956=DIRECTION('ref_axis',(1.22464679914735E-16,-1.,0.));
#20957=DIRECTION('center_axis',(-1.7238387684654E-15,-0.111847407981876,
-0.99372539331937));
#20958=DIRECTION('ref_axis',(-7.80419006320916E-33,0.99372539331937,-0.111847407981876));
#20959=DIRECTION('center_axis',(-1.,-1.22464679914735E-16,0.));
#20960=DIRECTION('ref_axis',(1.22464679914735E-16,-1.,0.));
#20961=DIRECTION('center_axis',(-2.42582538141765E-15,0.804667731009302,
0.593725393319455));
#20962=DIRECTION('ref_axis',(-5.51486489057277E-31,-0.593725393319454,0.804667731009302));
#20963=DIRECTION('center_axis',(1.,1.22464679914735E-16,0.));
#20964=DIRECTION('ref_axis',(-1.22464679914735E-16,1.,0.));
#20965=DIRECTION('center_axis',(-1.,0.,0.));
#20966=DIRECTION('ref_axis',(0.,0.,1.));
#20967=DIRECTION('',(-1.,-1.22464679914735E-16,0.));
#20968=DIRECTION('center_axis',(1.,0.,0.));
#20969=DIRECTION('ref_axis',(0.,0.,-1.));
#20970=DIRECTION('',(1.,1.22464679914735E-16,0.));
#20971=DIRECTION('center_axis',(1.,1.22464679914735E-16,0.));
#20972=DIRECTION('ref_axis',(-1.22464679914735E-16,1.,0.));
#20973=DIRECTION('',(1.,1.22464679914735E-16,0.));
#20974=DIRECTION('center_axis',(1.,1.22464679914735E-16,0.));
#20975=DIRECTION('ref_axis',(1.22464679914735E-16,-1.,0.));
#20976=DIRECTION('center_axis',(1.,1.22464679914735E-16,0.));
#20977=DIRECTION('ref_axis',(-1.22464679914735E-16,1.,0.));
#20978=DIRECTION('',(1.,1.22464679914735E-16,0.));
#20979=DIRECTION('center_axis',(1.,1.22464679914735E-16,0.));
#20980=DIRECTION('ref_axis',(1.22464679914735E-16,-1.,1.77635683940026E-15));
#20981=DIRECTION('center_axis',(1.,1.22464679914735E-16,0.));
#20982=DIRECTION('ref_axis',(-1.22464679914735E-16,1.,0.));
#20983=DIRECTION('',(1.,1.22464679914735E-16,0.));
#20984=DIRECTION('center_axis',(1.,1.22464679914735E-16,0.));
#20985=DIRECTION('ref_axis',(1.22464679914735E-16,-1.,1.15648231731769E-15));
#20986=DIRECTION('',(-1.,-1.22464679914735E-16,0.));
#20987=DIRECTION('center_axis',(-1.,-1.22464679914735E-16,0.));
#20988=DIRECTION('ref_axis',(1.22464679914735E-16,-1.,0.));
#20989=DIRECTION('center_axis',(-1.,-1.22464679914735E-16,0.));
#20990=DIRECTION('ref_axis',(1.22464679914735E-16,-1.,0.));
#20991=DIRECTION('',(-1.,-1.22464679914735E-16,0.));
#20992=DIRECTION('center_axis',(-1.,-1.22464679914735E-16,0.));
#20993=DIRECTION('ref_axis',(1.22464679914735E-16,-1.,0.));
#20994=DIRECTION('center_axis',(-1.,-1.22464679914735E-16,0.));
#20995=DIRECTION('ref_axis',(1.22464679914735E-16,-1.,0.));
#20996=DIRECTION('center_axis',(-1.,-1.22464679914735E-16,0.));
#20997=DIRECTION('ref_axis',(1.22464679914735E-16,-1.,0.));
#20998=DIRECTION('',(1.,1.22464679914735E-16,0.));
#20999=DIRECTION('center_axis',(-1.,-1.22464679914735E-16,0.));
#21000=DIRECTION('ref_axis',(1.22464679914735E-16,-1.,0.));
#21001=DIRECTION('center_axis',(-1.,-1.22464679914735E-16,0.));
#21002=DIRECTION('ref_axis',(1.22464679914735E-16,-1.,0.));
#21003=DIRECTION('center_axis',(1.,1.22464679914735E-16,0.));
#21004=DIRECTION('ref_axis',(-1.22464679914735E-16,1.,0.));
#21005=DIRECTION('',(1.,1.22464679914735E-16,0.));
#21006=DIRECTION('center_axis',(-1.,-1.22464679914735E-16,0.));
#21007=DIRECTION('ref_axis',(1.22464679914735E-16,-1.,0.));
#21008=DIRECTION('',(-1.,-1.22464679914735E-16,0.));
#21009=DIRECTION('center_axis',(-1.,-1.22464679914735E-16,0.));
#21010=DIRECTION('ref_axis',(1.22464679914735E-16,-1.,0.));
#21011=DIRECTION('center_axis',(1.,1.22464679914735E-16,0.));
#21012=DIRECTION('ref_axis',(-1.22464679914735E-16,1.,0.));
#21013=DIRECTION('',(1.,1.22464679914735E-16,0.));
#21014=DIRECTION('center_axis',(-1.,-1.22464679914735E-16,0.));
#21015=DIRECTION('ref_axis',(1.22464679914735E-16,-1.,0.));
#21016=DIRECTION('center_axis',(-1.,-1.22464679914735E-16,0.));
#21017=DIRECTION('ref_axis',(1.22464679914735E-16,-1.,0.));
#21018=DIRECTION('center_axis',(-1.,-1.22464679914735E-16,0.));
#21019=DIRECTION('ref_axis',(1.22464679914735E-16,-1.,0.));
#21020=DIRECTION('center_axis',(1.,1.22464679914735E-16,0.));
#21021=DIRECTION('ref_axis',(-1.22464679914735E-16,1.,0.));
#21022=DIRECTION('center_axis',(-1.,-1.22464679914735E-16,0.));
#21023=DIRECTION('ref_axis',(1.22464679914735E-16,-1.,0.));
#21024=DIRECTION('center_axis',(-1.,-1.22464679914735E-16,0.));
#21025=DIRECTION('ref_axis',(1.22464679914735E-16,-1.,0.));
#21026=DIRECTION('',(-1.,-1.22464679914735E-16,0.));
#21027=DIRECTION('center_axis',(1.,1.22464679914735E-16,0.));
#21028=DIRECTION('ref_axis',(-1.22464679914735E-16,1.,0.));
#21029=DIRECTION('center_axis',(-1.,-1.22464679914735E-16,0.));
#21030=DIRECTION('ref_axis',(1.22464679914735E-16,-1.,0.));
#21031=DIRECTION('center_axis',(-1.,-1.22464679914735E-16,0.));
#21032=DIRECTION('ref_axis',(1.22464679914735E-16,-1.,0.));
#21033=DIRECTION('',(-1.,-1.22464679914735E-16,0.));
#21034=DIRECTION('center_axis',(1.,1.22464679914735E-16,0.));
#21035=DIRECTION('ref_axis',(-1.22464679914735E-16,1.,0.));
#21036=DIRECTION('',(1.,1.22464679914735E-16,0.));
#21037=DIRECTION('center_axis',(1.,1.22464679914735E-16,0.));
#21038=DIRECTION('ref_axis',(-1.24344978758018E-16,1.,0.));
#21039=DIRECTION('center_axis',(-1.,-1.22464679914735E-16,0.));
#21040=DIRECTION('ref_axis',(-1.22464679914735E-16,1.,-7.99360577730113E-15));
#21041=DIRECTION('center_axis',(-8.10039603428687E-17,0.661447532458067,
-0.749991441154587));
#21042=DIRECTION('ref_axis',(-2.96250659143342E-32,-0.749991441154587,-0.661447532458067));
#21043=DIRECTION('center_axis',(3.90402550029783E-17,-0.318787874431711,
0.947826086956522));
#21044=DIRECTION('ref_axis',(-3.57000607053533E-33,-0.947826086956522,-0.318787874431711));
#21045=DIRECTION('center_axis',(1.,1.22464679914735E-16,0.));
#21046=DIRECTION('ref_axis',(-1.24344978758018E-16,1.,0.));
#21047=DIRECTION('center_axis',(-1.,-1.22464679914735E-16,0.));
#21048=DIRECTION('ref_axis',(-1.22464679914735E-16,1.,0.));
#21049=DIRECTION('center_axis',(3.90402550029783E-17,-0.318787874431711,
-0.947826086956522));
#21050=DIRECTION('ref_axis',(-3.57000607053533E-33,-0.947826086956522,0.318787874431711));
#21051=DIRECTION('center_axis',(-8.10039603428704E-17,0.661447532458081,
0.749991441154575));
#21052=DIRECTION('ref_axis',(7.37954811975299E-33,-0.749991441154575,0.661447532458081));
#21053=DIRECTION('center_axis',(1.,1.22464679914735E-16,0.));
#21054=DIRECTION('ref_axis',(-1.24344978758018E-16,1.,0.));
#21055=DIRECTION('center_axis',(1.20044215345851E-16,-0.980235406889814,
0.197834645801896));
#21056=DIRECTION('ref_axis',(-2.0076031589995E-32,-0.197834645801896,-0.980235406889814));
#21057=DIRECTION('center_axis',(-1.,-1.22464679914735E-16,0.));
#21058=DIRECTION('ref_axis',(-1.22464679914735E-16,1.,7.105427357601E-15));
#21059=DIRECTION('center_axis',(-1.20044215345851E-16,0.980235406889808,
0.197834645801926));
#21060=DIRECTION('ref_axis',(1.61897508715493E-32,0.197834645801926,-0.980235406889808));
#21061=DIRECTION('center_axis',(1.,1.22464679914735E-16,0.));
#21062=DIRECTION('ref_axis',(-1.24344978758018E-16,1.,0.));
#21063=DIRECTION('center_axis',(8.10039603428609E-17,-0.661447532458004,
-0.749991441154643));
#21064=DIRECTION('ref_axis',(7.96570883309855E-33,0.749991441154643,-0.661447532458004));
#21065=DIRECTION('center_axis',(-1.,-1.22464679914735E-16,0.));
#21066=DIRECTION('ref_axis',(-1.22464679914735E-16,1.,0.));
#21067=DIRECTION('center_axis',(-3.90402550029794E-17,0.31878787443172,
0.947826086956519));
#21068=DIRECTION('ref_axis',(2.68331918262955E-33,0.947826086956519,-0.31878787443172));
#21069=DIRECTION('center_axis',(1.,1.22464679914735E-16,0.));
#21070=DIRECTION('ref_axis',(-1.24344978758018E-16,1.,0.));
#21071=DIRECTION('center_axis',(1.,1.22464679914735E-16,0.));
#21072=DIRECTION('ref_axis',(-1.22464679914735E-16,1.,0.));
#21073=DIRECTION('center_axis',(-1.20044215345852E-16,0.980235406889816,
-0.197834645801884));
#21074=DIRECTION('ref_axis',(-2.66733220812947E-32,0.197834645801884,0.980235406889816));
#21075=DIRECTION('center_axis',(-1.,-1.22464679914735E-16,0.));
#21076=DIRECTION('ref_axis',(-1.22464679914735E-16,1.,0.));
#21077=DIRECTION('center_axis',(1.20044215345849E-16,-0.980235406889798,
-0.197834645801971));
#21078=DIRECTION('ref_axis',(-7.95464076645661E-33,-0.197834645801971,0.980235406889798));
#21079=DIRECTION('center_axis',(-1.,-1.22464679914735E-16,0.));
#21080=DIRECTION('ref_axis',(1.4210854715202E-16,-1.,0.));
#21081=DIRECTION('center_axis',(-8.10039603428687E-17,0.661447532458067,
-0.749991441154587));
#21082=DIRECTION('ref_axis',(-2.27599120852545E-32,0.749991441154587,0.661447532458068));
#21083=DIRECTION('center_axis',(1.,1.22464679914735E-16,0.));
#21084=DIRECTION('ref_axis',(1.22464679914735E-16,-1.,0.));
#21085=DIRECTION('center_axis',(3.90402550029783E-17,-0.318787874431711,
0.947826086956522));
#21086=DIRECTION('ref_axis',(1.97143231695727E-32,0.947826086956522,0.318787874431711));
#21087=DIRECTION('center_axis',(-1.,-1.22464679914735E-16,0.));
#21088=DIRECTION('ref_axis',(1.4210854715202E-16,-1.,0.));
#21089=DIRECTION('center_axis',(3.90402550029783E-17,-0.318787874431711,
-0.947826086956522));
#21090=DIRECTION('ref_axis',(1.97143231695727E-32,0.947826086956522,-0.318787874431711));
#21091=DIRECTION('center_axis',(1.,1.22464679914735E-16,0.));
#21092=DIRECTION('ref_axis',(1.22464679914735E-16,-1.,-2.66453525910038E-15));
#21093=DIRECTION('center_axis',(-8.10039603428704E-17,0.661447532458081,
0.749991441154575));
#21094=DIRECTION('ref_axis',(2.2108738618768E-32,0.749991441154575,-0.661447532458081));
#21095=DIRECTION('center_axis',(-1.,-1.22464679914735E-16,0.));
#21096=DIRECTION('ref_axis',(1.4210854715202E-16,-1.,0.));
#21097=DIRECTION('center_axis',(1.,1.22464679914735E-16,0.));
#21098=DIRECTION('ref_axis',(1.22464679914735E-16,-1.,7.105427357601E-15));
#21099=DIRECTION('center_axis',(1.20044215345851E-16,-0.980235406889814,
0.197834645801896));
#21100=DIRECTION('ref_axis',(2.0076031589995E-32,0.197834645801896,0.980235406889814));
#21101=DIRECTION('center_axis',(-1.20044215345851E-16,0.980235406889808,
0.197834645801926));
#21102=DIRECTION('ref_axis',(-1.61897508715493E-32,-0.197834645801926,0.980235406889808));
#21103=DIRECTION('center_axis',(-1.,-1.22464679914735E-16,0.));
#21104=DIRECTION('ref_axis',(1.4210854715202E-16,-1.,0.));
#21105=DIRECTION('center_axis',(1.,1.22464679914735E-16,0.));
#21106=DIRECTION('ref_axis',(1.22464679914735E-16,-1.,1.77635683940025E-15));
#21107=DIRECTION('center_axis',(8.10039603428609E-17,-0.661447532458004,
-0.749991441154643));
#21108=DIRECTION('ref_axis',(-5.20417042793042E-15,-0.749991441154643,0.661447532458004));
#21109=DIRECTION('center_axis',(-3.90402550029794E-17,0.31878787443172,
0.947826086956519));
#21110=DIRECTION('ref_axis',(-2.68331918262955E-33,-0.947826086956519,0.31878787443172));
#21111=DIRECTION('center_axis',(-1.,-1.22464679914735E-16,0.));
#21112=DIRECTION('ref_axis',(1.4210854715202E-16,-1.,0.));
#21113=DIRECTION('center_axis',(1.,1.22464679914735E-16,0.));
#21114=DIRECTION('ref_axis',(1.22464679914735E-16,-1.,0.));
#21115=DIRECTION('center_axis',(-1.20044215345852E-16,0.980235406889816,
-0.197834645801884));
#21116=DIRECTION('ref_axis',(2.66733220812947E-32,-0.197834645801884,-0.980235406889816));
#21117=DIRECTION('center_axis',(-1.,-1.22464679914735E-16,0.));
#21118=DIRECTION('ref_axis',(1.22464679914735E-16,-1.,0.));
#21119=DIRECTION('center_axis',(1.20044215345849E-16,-0.980235406889798,
-0.197834645801971));
#21120=DIRECTION('ref_axis',(7.95464076645661E-33,0.197834645801971,-0.980235406889798));
#21121=DIRECTION('center_axis',(1.,1.22464679914735E-16,0.));
#21122=DIRECTION('ref_axis',(-1.22464679914735E-16,1.,0.));
#21123=DIRECTION('center_axis',(1.,1.22464679914735E-16,0.));
#21124=DIRECTION('ref_axis',(-1.22464679914735E-16,1.,0.));
#21125=DIRECTION('center_axis',(1.,1.22464679914735E-16,0.));
#21126=DIRECTION('ref_axis',(-1.22464679914735E-16,1.,0.));
#21127=DIRECTION('center_axis',(1.,1.22464679914735E-16,0.));
#21128=DIRECTION('ref_axis',(-1.22464679914735E-16,1.,0.));
#21129=DIRECTION('center_axis',(-1.,-1.22464679914735E-16,0.));
#21130=DIRECTION('ref_axis',(-1.22464679914735E-16,1.,0.));
#21131=DIRECTION('center_axis',(-1.,-1.22464679914735E-16,0.));
#21132=DIRECTION('ref_axis',(1.22464679914735E-16,-1.,0.));
#21133=DIRECTION('',(-1.,-1.22464679914735E-16,0.));
#21134=DIRECTION('',(1.,1.22464679914735E-16,0.));
#21135=DIRECTION('center_axis',(-1.,-1.22464679914735E-16,0.));
#21136=DIRECTION('ref_axis',(1.22464679914735E-16,-1.,0.));
#21137=DIRECTION('center_axis',(-1.,-1.22464679914735E-16,0.));
#21138=DIRECTION('ref_axis',(1.22464679914735E-16,-1.,0.));
#21139=DIRECTION('center_axis',(-1.,-1.22464679914735E-16,0.));
#21140=DIRECTION('ref_axis',(1.22464679914735E-16,-1.,0.));
#21141=DIRECTION('center_axis',(1.,1.22464679914735E-16,0.));
#21142=DIRECTION('ref_axis',(1.22464679914735E-16,-1.,0.));
#21143=DIRECTION('center_axis',(-1.,-1.22464679914735E-16,0.));
#21144=DIRECTION('ref_axis',(1.22464679914735E-16,-1.,0.));
#21145=DIRECTION('center_axis',(-1.,-1.22464679914735E-16,0.));
#21146=DIRECTION('ref_axis',(1.22464679914735E-16,-1.,0.));
#21147=DIRECTION('center_axis',(-1.,-1.22464679914735E-16,0.));
#21148=DIRECTION('ref_axis',(1.22464679914735E-16,-1.,0.));
#21149=DIRECTION('center_axis',(1.,1.22464679914735E-16,0.));
#21150=DIRECTION('ref_axis',(-1.24344978758018E-16,1.,0.));
#21151=DIRECTION('center_axis',(-3.90402550029925E-17,0.318787874431827,
-0.947826086956483));
#21152=DIRECTION('ref_axis',(-6.44688282815806E-33,0.947826086956483,0.318787874431827));
#21153=DIRECTION('center_axis',(8.10039603428727E-17,-0.6614475324581,0.749991441154558));
#21154=DIRECTION('ref_axis',(-3.97296770160977E-32,0.749991441154558,0.6614475324581));
#21155=DIRECTION('center_axis',(-1.,-1.22464679914735E-16,0.));
#21156=DIRECTION('ref_axis',(1.4210854715202E-16,-1.,0.));
#21157=DIRECTION('center_axis',(-3.90402550029925E-17,0.318787874431827,
-0.947826086956483));
#21158=DIRECTION('ref_axis',(-1.26985355407412E-32,-0.947826086956483,-0.318787874431827));
#21159=DIRECTION('center_axis',(8.10039603428727E-17,-0.6614475324581,0.749991441154558));
#21160=DIRECTION('ref_axis',(3.97296770160977E-32,-0.749991441154558,-0.6614475324581));
#21161=DIRECTION('center_axis',(1.,1.22464679914735E-16,0.));
#21162=DIRECTION('ref_axis',(6.12323399573693E-17,-0.500000000000013,0.866025403784431));
#21163=DIRECTION('',(-1.,-1.22464679914735E-16,0.));
#21164=DIRECTION('center_axis',(-1.,-1.22464679914735E-16,0.));
#21165=DIRECTION('ref_axis',(-1.22464679914735E-16,1.,1.15648231731783E-15));
#21166=DIRECTION('',(1.,1.22464679914735E-16,0.));
#21167=DIRECTION('center_axis',(1.,1.22464679914735E-16,0.));
#21168=DIRECTION('ref_axis',(6.12323399573661E-17,-0.499999999999987,-0.866025403784446));
#21169=DIRECTION('',(-1.,-1.22464679914735E-16,0.));
#21170=DIRECTION('center_axis',(-1.,-1.22464679914735E-16,0.));
#21171=DIRECTION('ref_axis',(-1.22464679914735E-16,1.,1.15648231731771E-15));
#21172=DIRECTION('center_axis',(1.,1.22464679914735E-16,0.));
#21173=DIRECTION('ref_axis',(1.22464679914735E-16,-1.,-1.22464679914735E-16));
#21174=DIRECTION('',(-1.,-1.22464679914735E-16,0.));
#21175=DIRECTION('center_axis',(-1.,-1.22464679914735E-16,0.));
#21176=DIRECTION('ref_axis',(-1.22464679914735E-16,1.,8.88178419700125E-16));
#21177=DIRECTION('center_axis',(1.,0.,0.));
#21178=DIRECTION('ref_axis',(0.,-0.111847407981875,-0.99372539331937));
#21179=DIRECTION('center_axis',(0.,-0.111847407981874,-0.99372539331937));
#21180=DIRECTION('ref_axis',(0.,0.99372539331937,-0.111847407981874));
#21181=DIRECTION('center_axis',(1.,0.,0.));
#21182=DIRECTION('ref_axis',(0.,-0.111847407981875,-0.99372539331937));
#21183=DIRECTION('center_axis',(1.,1.22464679914735E-16,0.));
#21184=DIRECTION('ref_axis',(4.44089209850026E-17,-0.499999999999987,-0.866025403784446));
#21185=DIRECTION('center_axis',(0.,0.804667731009303,0.593725393319454));
#21186=DIRECTION('ref_axis',(0.,-0.593725393319454,0.804667731009303));
#21187=DIRECTION('center_axis',(1.,0.,0.));
#21188=DIRECTION('ref_axis',(0.,0.804667731009302,0.593725393319455));
#21189=DIRECTION('center_axis',(1.,0.,0.));
#21190=DIRECTION('ref_axis',(0.,0.,-1.));
#21191=DIRECTION('center_axis',(1.,0.,0.));
#21192=DIRECTION('ref_axis',(0.,0.804667731009302,0.593725393319455));
#21193=DIRECTION('center_axis',(-1.,0.,0.));
#21194=DIRECTION('ref_axis',(0.,0.,1.));
#21195=DIRECTION('center_axis',(-1.,-1.22464679914735E-16,0.));
#21196=DIRECTION('ref_axis',(1.22464679914735E-16,-1.,0.));
#21197=DIRECTION('center_axis',(1.,1.22464679914735E-16,0.));
#21198=DIRECTION('ref_axis',(-1.22464679914735E-16,1.,0.));
#21199=DIRECTION('center_axis',(-1.,0.,0.));
#21200=DIRECTION('ref_axis',(0.,0.,1.));
#21201=DIRECTION('center_axis',(1.,0.,0.));
#21202=DIRECTION('ref_axis',(0.,0.,-1.));
#21203=DIRECTION('center_axis',(1.,0.,0.));
#21204=DIRECTION('ref_axis',(0.,0.804667731009333,-0.593725393319414));
#21205=DIRECTION('center_axis',(1.,0.,0.));
#21206=DIRECTION('ref_axis',(0.,0.804667731009332,-0.593725393319415));
#21207=DIRECTION('center_axis',(-1.91085069238026E-15,0.804667731009333,
-0.593725393319414));
#21208=DIRECTION('ref_axis',(2.55801177487293E-31,0.593725393319413,0.804667731009333));
#21209=DIRECTION('center_axis',(-1.,-1.22464679914735E-16,0.));
#21210=DIRECTION('ref_axis',(0.,0.500000000000037,-0.866025403784417));
#21211=DIRECTION('center_axis',(1.62682660628867E-15,-0.11184740798194,
0.993725393319362));
#21212=DIRECTION('ref_axis',(8.0958773252926E-32,-0.993725393319362,-0.11184740798194));
#21213=DIRECTION('center_axis',(1.,0.,0.));
#21214=DIRECTION('ref_axis',(0.,-0.111847407981939,0.993725393319362));
#21215=DIRECTION('center_axis',(1.,0.,0.));
#21216=DIRECTION('ref_axis',(0.,-0.111847407981939,0.993725393319362));
#21217=DIRECTION('center_axis',(1.,1.22464679914735E-16,0.));
#21218=DIRECTION('ref_axis',(1.11949878192378E-16,-0.914140128160396,0.405398354815231));
#21219=DIRECTION('center_axis',(-1.,-1.99493199737328E-16,-8.70659703262238E-17));
#21220=DIRECTION('ref_axis',(1.99493199737328E-16,-1.,-1.51035382683644E-33));
#21221=DIRECTION('center_axis',(1.,0.,0.));
#21222=DIRECTION('ref_axis',(0.,0.,-1.));
#21223=DIRECTION('center_axis',(1.,0.,0.));
#21224=DIRECTION('ref_axis',(0.,0.916515138991152,0.400000000000037));
#21225=DIRECTION('center_axis',(1.,0.,0.));
#21226=DIRECTION('ref_axis',(0.,0.916515138991152,0.400000000000037));
#21227=DIRECTION('center_axis',(0.,0.916515138991152,0.400000000000037));
#21228=DIRECTION('ref_axis',(0.,-0.400000000000037,0.916515138991152));
#21229=DIRECTION('center_axis',(-1.,-1.22464679914735E-16,0.));
#21230=DIRECTION('ref_axis',(-1.77635683939998E-16,1.,5.67209541808933E-14));
#21231=DIRECTION('center_axis',(3.46944695195304E-16,-0.916515138991197,
0.399999999999933));
#21232=DIRECTION('ref_axis',(-7.5199079965689E-34,-0.399999999999933,-0.916515138991197));
#21233=DIRECTION('center_axis',(1.,0.,0.));
#21234=DIRECTION('ref_axis',(0.,-0.916515138991197,0.399999999999933));
#21235=DIRECTION('center_axis',(1.,0.,0.));
#21236=DIRECTION('ref_axis',(0.,-0.916515138991197,0.399999999999933));
#21237=DIRECTION('center_axis',(-1.,-1.22464679914735E-16,0.));
#21238=DIRECTION('ref_axis',(0.,0.499999999999963,0.86602540378446));
#21239=DIRECTION('center_axis',(0.,-0.111847407981704,-0.993725393319389));
#21240=DIRECTION('ref_axis',(0.,0.993725393319389,-0.111847407981704));
#21241=DIRECTION('center_axis',(2.42582538141761E-15,-0.804667731009371,
-0.593725393319361));
#21242=DIRECTION('ref_axis',(-2.98202186050019E-31,0.593725393319361,-0.804667731009371));
#21243=DIRECTION('center_axis',(1.,4.44089209850063E-16,0.));
#21244=DIRECTION('ref_axis',(0.,0.111847407981704,0.993725393319389));
#21245=DIRECTION('center_axis',(-1.,0.,0.));
#21246=DIRECTION('ref_axis',(0.,0.,1.));
#21247=DIRECTION('center_axis',(1.,0.,0.));
#21248=DIRECTION('ref_axis',(0.,-0.804667731009372,-0.593725393319361));
#21249=DIRECTION('center_axis',(-1.,0.,0.));
#21250=DIRECTION('ref_axis',(0.,0.,1.));
#21251=DIRECTION('center_axis',(1.,1.22464679914735E-16,0.));
#21252=DIRECTION('ref_axis',(9.8970484789873E-17,-0.808155338002599,-0.588969396198059));
#21253=DIRECTION('center_axis',(-1.,0.,0.));
#21254=DIRECTION('ref_axis',(0.,0.,1.));
#21255=DIRECTION('center_axis',(-1.,-1.22464679914735E-16,0.));
#21256=DIRECTION('ref_axis',(1.22464679914735E-16,-1.,0.));
#21257=DIRECTION('center_axis',(-1.,0.,0.));
#21258=DIRECTION('ref_axis',(0.,0.,1.));
#21259=DIRECTION('center_axis',(1.,0.,0.));
#21260=DIRECTION('ref_axis',(0.,0.111847407981704,0.993725393319389));
#21261=DIRECTION('center_axis',(1.,0.,0.));
#21262=DIRECTION('ref_axis',(0.,-0.804667731009372,-0.593725393319361));
#21263=DIRECTION('center_axis',(1.,0.,0.));
#21264=DIRECTION('ref_axis',(0.,-0.916515138991168,-0.400000000000001));
#21265=DIRECTION('center_axis',(1.,0.,0.));
#21266=DIRECTION('ref_axis',(0.,0.916515138991168,-0.400000000000001));
#21267=DIRECTION('center_axis',(-1.,0.,0.));
#21268=DIRECTION('ref_axis',(0.,0.,1.));
#21269=DIRECTION('center_axis',(-1.,-1.22464679914735E-16,0.));
#21270=DIRECTION('ref_axis',(-1.11949878192374E-16,0.914140128160362,0.405398354815307));
#21271=DIRECTION('center_axis',(-1.,-1.99493199737332E-16,8.70659703262165E-17));
#21272=DIRECTION('ref_axis',(1.99493199737332E-16,-1.,1.51035382683594E-33));
#21273=DIRECTION('center_axis',(1.,0.,0.));
#21274=DIRECTION('ref_axis',(0.,-0.916515138991168,-0.400000000000001));
#21275=DIRECTION('center_axis',(0.,-0.916515138991168,-0.4));
#21276=DIRECTION('ref_axis',(0.,0.4,-0.916515138991168));
#21277=DIRECTION('center_axis',(1.,0.,0.));
#21278=DIRECTION('ref_axis',(0.,0.916515138991168,-0.400000000000001));
#21279=DIRECTION('center_axis',(-1.24295563250076E-15,-0.916515138991168,
0.400000000000001));
#21280=DIRECTION('ref_axis',(7.88837516234267E-32,-0.400000000000001,-0.916515138991168));
#21281=DIRECTION('center_axis',(1.,1.22464679914735E-16,0.));
#21282=DIRECTION('ref_axis',(1.11022302462516E-16,-1.,1.22464679914735E-16));
#21283=DIRECTION('center_axis',(1.,0.,0.));
#21284=DIRECTION('ref_axis',(0.,-0.804667731009409,0.59372539331931));
#21285=DIRECTION('center_axis',(-1.,0.,0.));
#21286=DIRECTION('ref_axis',(0.,0.,1.));
#21287=DIRECTION('center_axis',(1.,4.44089209850063E-16,0.));
#21288=DIRECTION('ref_axis',(0.,0.111847407981753,-0.993725393319383));
#21289=DIRECTION('center_axis',(-1.,0.,0.));
#21290=DIRECTION('ref_axis',(0.,0.,1.));
#21291=DIRECTION('center_axis',(1.,1.22464679914735E-16,0.));
#21292=DIRECTION('ref_axis',(-1.22464679914735E-16,1.,0.));
#21293=DIRECTION('center_axis',(-1.,0.,0.));
#21294=DIRECTION('ref_axis',(0.,0.,1.));
#21295=DIRECTION('center_axis',(-1.,-1.22464679914735E-16,0.));
#21296=DIRECTION('ref_axis',(-9.89704847898782E-17,0.808155338002642,-0.588969396197999));
#21297=DIRECTION('center_axis',(-1.,-2.13362867122436E-16,-4.30616635022305E-17));
#21298=DIRECTION('ref_axis',(2.13362867122436E-16,-1.,-1.49749836094163E-34));
#21299=DIRECTION('center_axis',(1.,0.,0.));
#21300=DIRECTION('ref_axis',(0.,-0.804667731009409,0.59372539331931));
#21301=DIRECTION('center_axis',(0.,-0.804667731009409,0.59372539331931));
#21302=DIRECTION('ref_axis',(0.,-0.59372539331931,-0.804667731009409));
#21303=DIRECTION('center_axis',(1.,0.,0.));
#21304=DIRECTION('ref_axis',(0.,0.111847407981753,-0.993725393319383));
#21305=DIRECTION('center_axis',(0.,-0.111847407981753,0.993725393319383));
#21306=DIRECTION('ref_axis',(0.,-0.993725393319383,-0.111847407981753));
#21307=DIRECTION('center_axis',(1.,1.22464679914735E-16,0.));
#21308=DIRECTION('ref_axis',(4.44089209850053E-17,-0.500000000000013,0.866025403784431));
#21309=DIRECTION('axis',(0.,0.,1.));
#21310=DIRECTION('refdir',(1.,0.,0.));
#21311=DIRECTION('center_axis',(0.,1.,0.));
#21312=DIRECTION('ref_axis',(0.,0.,1.));
#21313=DIRECTION('center_axis',(0.,1.,0.));
#21314=DIRECTION('ref_axis',(0.,0.,-1.));
#21315=DIRECTION('',(-8.65956056235501E-17,0.707106781186541,-0.707106781186554));
#21316=DIRECTION('center_axis',(0.,-1.,0.));
#21317=DIRECTION('ref_axis',(0.,0.,-1.));
#21318=DIRECTION('center_axis',(0.,0.,1.));
#21319=DIRECTION('ref_axis',(1.,0.,0.));
#21320=DIRECTION('center_axis',(0.,0.,1.));
#21321=DIRECTION('ref_axis',(-1.,0.,0.));
#21322=DIRECTION('center_axis',(0.,0.,1.));
#21323=DIRECTION('ref_axis',(-1.,0.,0.));
#21324=DIRECTION('',(-0.707106781186545,-8.6595605623549E-17,0.70710678118655));
#21325=DIRECTION('center_axis',(-1.22464679914735E-16,0.,-1.));
#21326=DIRECTION('ref_axis',(-1.,0.,1.22464679914735E-16));
#21327=DIRECTION('center_axis',(0.,0.,1.));
#21328=DIRECTION('ref_axis',(1.,0.,0.));
#21329=DIRECTION('center_axis',(0.,0.,1.));
#21330=DIRECTION('ref_axis',(-1.,0.,0.));
#21331=DIRECTION('center_axis',(0.,0.,1.));
#21332=DIRECTION('ref_axis',(-1.,0.,0.));
#21333=DIRECTION('',(-0.707106781186547,-8.65956056235493E-17,0.707106781186548));
#21334=DIRECTION('center_axis',(-1.22464679914735E-16,0.,-1.));
#21335=DIRECTION('ref_axis',(-1.,0.,1.22464679914735E-16));
#21336=DIRECTION('center_axis',(0.,1.,0.));
#21337=DIRECTION('ref_axis',(0.,0.,1.));
#21338=DIRECTION('center_axis',(0.,1.,0.));
#21339=DIRECTION('ref_axis',(0.,0.,-1.));
#21340=DIRECTION('',(-8.65956056235498E-17,0.707106781186544,-0.707106781186551));
#21341=DIRECTION('center_axis',(0.,-1.,0.));
#21342=DIRECTION('ref_axis',(0.,0.,-1.));
#21343=DIRECTION('center_axis',(0.,0.,1.));
#21344=DIRECTION('ref_axis',(0.81777431008862,-0.575539032350614,0.));
#21345=DIRECTION('center_axis',(0.,0.,1.));
#21346=DIRECTION('ref_axis',(-1.,0.,0.));
#21347=DIRECTION('center_axis',(7.03266274044652E-17,0.,-1.));
#21348=DIRECTION('ref_axis',(-1.,0.,-7.03266274044651E-17));
#21349=DIRECTION('center_axis',(0.,-1.,0.));
#21350=DIRECTION('ref_axis',(0.,0.,-1.));
#21351=DIRECTION('center_axis',(0.,-1.,0.));
#21352=DIRECTION('ref_axis',(0.,0.,1.));
#21353=DIRECTION('center_axis',(0.,-1.,0.));
#21354=DIRECTION('ref_axis',(0.,0.,1.));
#21355=DIRECTION('',(-8.65956056235497E-17,-0.707106781186545,0.70710678118655));
#21356=DIRECTION('center_axis',(0.,1.,0.));
#21357=DIRECTION('ref_axis',(0.,0.,1.));
#21358=DIRECTION('center_axis',(0.,-1.,0.));
#21359=DIRECTION('ref_axis',(0.,0.,-1.));
#21360=DIRECTION('center_axis',(0.,-1.,0.));
#21361=DIRECTION('ref_axis',(0.,0.,-1.));
#21362=DIRECTION('center_axis',(0.,-1.,0.));
#21363=DIRECTION('ref_axis',(0.,0.,-1.));
#21364=DIRECTION('',(-8.6595605623549E-17,-0.707106781186551,0.707106781186544));
#21365=DIRECTION('center_axis',(0.,1.,0.));
#21366=DIRECTION('ref_axis',(0.,0.,-1.));
#21367=DIRECTION('center_axis',(0.,0.,-1.));
#21368=DIRECTION('ref_axis',(-1.,0.,0.));
#21369=DIRECTION('center_axis',(0.,0.,-1.));
#21370=DIRECTION('ref_axis',(1.,0.,0.));
#21371=DIRECTION('',(0.707106781186542,-8.65956056235487E-17,-0.707106781186553));
#21372=DIRECTION('center_axis',(0.,0.,1.));
#21373=DIRECTION('ref_axis',(1.,0.,0.));
#21374=DIRECTION('center_axis',(0.,0.,-1.));
#21375=DIRECTION('ref_axis',(-1.,0.,0.));
#21376=DIRECTION('center_axis',(0.,0.,-1.));
#21377=DIRECTION('ref_axis',(1.,0.,0.));
#21378=DIRECTION('',(0.707106781186544,-8.65956056235489E-17,-0.707106781186551));
#21379=DIRECTION('center_axis',(0.,0.,1.));
#21380=DIRECTION('ref_axis',(1.,0.,0.));
#21381=DIRECTION('center_axis',(0.,0.,-1.));
#21382=DIRECTION('ref_axis',(0.817774310088624,-0.575539032350609,0.));
#21383=DIRECTION('center_axis',(0.,0.,-1.));
#21384=DIRECTION('ref_axis',(1.,0.,0.));
#21385=DIRECTION('center_axis',(0.,0.,1.));
#21386=DIRECTION('ref_axis',(1.,0.,0.));
#21387=DIRECTION('center_axis',(0.,1.,0.));
#21388=DIRECTION('ref_axis',(0.,0.,1.));
#21389=DIRECTION('',(0.,1.,0.));
#21390=DIRECTION('center_axis',(0.,-1.,0.));
#21391=DIRECTION('ref_axis',(0.,0.,-1.));
#21392=DIRECTION('center_axis',(0.,-1.,0.));
#21393=DIRECTION('ref_axis',(0.,0.,-1.));
#21394=DIRECTION('center_axis',(0.,1.,0.));
#21395=DIRECTION('ref_axis',(0.,0.,1.));
#21396=DIRECTION('center_axis',(0.,1.,0.));
#21397=DIRECTION('ref_axis',(0.,0.,1.));
#21398=DIRECTION('',(0.,1.,0.));
#21399=DIRECTION('center_axis',(0.,1.,0.));
#21400=DIRECTION('ref_axis',(0.,0.,1.));
#21401=DIRECTION('',(0.,1.,0.));
#21402=DIRECTION('center_axis',(0.,0.,-1.));
#21403=DIRECTION('ref_axis',(0.782779647501618,-0.622298982368798,0.));
#21404=DIRECTION('',(0.,0.,-1.));
#21405=DIRECTION('',(0.,0.,-1.));
#21406=DIRECTION('',(0.,0.,-1.));
#21407=DIRECTION('center_axis',(0.,0.,-1.));
#21408=DIRECTION('ref_axis',(-1.,0.,0.));
#21409=DIRECTION('',(0.,0.,-1.));
#21410=DIRECTION('center_axis',(0.,0.,-1.));
#21411=DIRECTION('ref_axis',(-1.,0.,0.));
#21412=DIRECTION('',(0.,0.,-1.));
#21413=DIRECTION('center_axis',(1.,0.,0.));
#21414=DIRECTION('ref_axis',(0.,0.,-1.));
#21415=DIRECTION('',(0.,-1.,0.));
#21416=DIRECTION('',(0.,0.,-1.));
#21417=DIRECTION('',(0.,-1.,0.));
#21418=DIRECTION('',(0.,0.,-1.));
#21419=DIRECTION('center_axis',(-1.,0.,0.));
#21420=DIRECTION('ref_axis',(0.,0.,1.));
#21421=DIRECTION('',(0.,0.,1.));
#21422=DIRECTION('',(0.,-1.,0.));
#21423=DIRECTION('',(0.,0.,-1.));
#21424=DIRECTION('',(0.,1.,0.));
#21425=DIRECTION('center_axis',(0.,0.,1.));
#21426=DIRECTION('ref_axis',(1.,0.,0.));
#21427=DIRECTION('',(1.,0.,0.));
#21428=DIRECTION('center_axis',(0.,0.,1.));
#21429=DIRECTION('ref_axis',(1.,0.,0.));
#21430=DIRECTION('',(1.,-3.62769940560266E-16,0.));
#21431=DIRECTION('',(0.,-1.,0.));
#21432=DIRECTION('',(0.866013897511261,0.500019928920193,0.));
#21433=DIRECTION('',(1.,0.,0.));
#21434=DIRECTION('',(0.,-1.,0.));
#21435=DIRECTION('',(-1.,0.,0.));
#21436=DIRECTION('',(0.,-1.,0.));
#21437=DIRECTION('',(-0.866013897511262,0.500019928920192,0.));
#21438=DIRECTION('',(0.,-1.,0.));
#21439=DIRECTION('',(-1.,7.25539881120531E-16,0.));
#21440=DIRECTION('center_axis',(0.,0.,1.));
#21441=DIRECTION('ref_axis',(1.,0.,0.));
#21442=DIRECTION('',(-1.,0.,0.));
#21443=DIRECTION('center_axis',(1.,0.,0.));
#21444=DIRECTION('ref_axis',(0.,0.,-1.));
#21445=DIRECTION('',(0.,0.,1.));
#21446=DIRECTION('',(0.,-1.,0.));
#21447=DIRECTION('',(0.,0.,-1.));
#21448=DIRECTION('center_axis',(7.03266274044652E-17,0.,-1.));
#21449=DIRECTION('ref_axis',(-1.,0.,-7.03266274044652E-17));
#21450=DIRECTION('',(1.,0.,0.));
#21451=DIRECTION('',(-1.,0.,0.));
#21452=DIRECTION('center_axis',(7.03266274044652E-17,0.,-1.));
#21453=DIRECTION('ref_axis',(-1.,0.,-7.03266274044652E-17));
#21454=DIRECTION('',(-1.,7.25539881120531E-16,0.));
#21455=DIRECTION('',(0.,-1.,0.));
#21456=DIRECTION('',(-0.866013897511262,0.500019928920192,0.));
#21457=DIRECTION('',(1.,0.,7.03266274044652E-17));
#21458=DIRECTION('',(0.,1.,0.));
#21459=DIRECTION('',(1.,0.,7.03266274044652E-17));
#21460=DIRECTION('',(0.,1.,0.));
#21461=DIRECTION('',(-1.,0.,-7.03266274044652E-17));
#21462=DIRECTION('',(0.,1.,0.));
#21463=DIRECTION('',(-1.,0.,-7.03266274044652E-17));
#21464=DIRECTION('',(0.866013897511261,0.500019928920193,0.));
#21465=DIRECTION('',(0.,-1.,0.));
#21466=DIRECTION('',(1.,-3.62769940560266E-16,0.));
#21467=DIRECTION('center_axis',(7.03266274044652E-17,0.,-1.));
#21468=DIRECTION('ref_axis',(-1.,0.,-7.03266274044652E-17));
#21469=DIRECTION('center_axis',(-1.,0.,0.));
#21470=DIRECTION('ref_axis',(0.,0.,1.));
#21471=DIRECTION('',(0.,0.,1.));
#21472=DIRECTION('',(0.,-1.,0.));
#21473=DIRECTION('',(0.,0.,-1.));
#21474=DIRECTION('',(0.,-1.,0.));
#21475=DIRECTION('center_axis',(-1.22464679914735E-16,0.,-1.));
#21476=DIRECTION('ref_axis',(-1.,0.,1.22464679914735E-16));
#21477=DIRECTION('',(0.,-1.,0.));
#21478=DIRECTION('',(1.,0.,-1.22464679914735E-16));
#21479=DIRECTION('',(0.,1.,0.));
#21480=DIRECTION('',(-1.,0.,1.22464679914735E-16));
#21481=DIRECTION('',(0.,1.,0.));
#21482=DIRECTION('',(-1.,0.,0.));
#21483=DIRECTION('',(1.,0.,-1.22464679914735E-16));
#21484=DIRECTION('center_axis',(0.,-1.,0.));
#21485=DIRECTION('ref_axis',(0.,0.,-1.));
#21486=DIRECTION('',(-1.,0.,0.));
#21487=DIRECTION('',(0.,0.,1.));
#21488=DIRECTION('',(1.,0.,7.03266274044652E-17));
#21489=DIRECTION('',(0.,0.,-1.));
#21490=DIRECTION('center_axis',(0.,-1.,0.));
#21491=DIRECTION('ref_axis',(0.,0.,-1.));
#21492=DIRECTION('',(1.,0.,-1.22464679914735E-16));
#21493=DIRECTION('',(0.,0.,-1.));
#21494=DIRECTION('center_axis',(0.,-1.,0.));
#21495=DIRECTION('ref_axis',(0.,0.,-1.));
#21496=DIRECTION('',(0.,0.,1.));
#21497=DIRECTION('',(-1.,0.,1.22464679914735E-16));
#21498=DIRECTION('',(0.,0.,-1.));
#21499=DIRECTION('',(-1.,0.,0.));
#21500=DIRECTION('center_axis',(0.,1.,0.));
#21501=DIRECTION('ref_axis',(0.,0.,-1.));
#21502=DIRECTION('',(0.,0.,1.));
#21503=DIRECTION('',(-1.,0.,-7.03266274044652E-17));
#21504=DIRECTION('',(0.,0.,-1.));
#21505=DIRECTION('',(1.,0.,0.));
#21506=DIRECTION('center_axis',(0.,0.,-1.));
#21507=DIRECTION('ref_axis',(-1.,0.,0.));
#21508=DIRECTION('',(0.,0.,-1.));
#21509=DIRECTION('center_axis',(0.,0.,-1.));
#21510=DIRECTION('ref_axis',(1.,0.,0.));
#21511=DIRECTION('',(0.,0.,-1.));
#21512=DIRECTION('center_axis',(0.,0.,1.));
#21513=DIRECTION('ref_axis',(-1.,0.,0.));
#21514=DIRECTION('center_axis',(0.,-1.,0.));
#21515=DIRECTION('ref_axis',(0.,0.,-1.));
#21516=DIRECTION('center_axis',(0.,1.,0.));
#21517=DIRECTION('ref_axis',(0.,0.,1.));
#21518=DIRECTION('',(0.,0.,-1.));
#21519=DIRECTION('center_axis',(0.,0.,-1.));
#21520=DIRECTION('ref_axis',(-1.,0.,0.));
#21521=DIRECTION('',(0.,0.,-1.));
#21522=DIRECTION('center_axis',(0.,0.,-1.));
#21523=DIRECTION('ref_axis',(1.,0.,0.));
#21524=DIRECTION('center_axis',(0.,0.,1.));
#21525=DIRECTION('ref_axis',(-1.,0.,0.));
#21526=DIRECTION('center_axis',(3.62769940560266E-16,1.,0.));
#21527=DIRECTION('ref_axis',(-1.,3.62769940560266E-16,0.));
#21528=DIRECTION('',(0.,0.,-1.));
#21529=DIRECTION('center_axis',(1.,0.,0.));
#21530=DIRECTION('ref_axis',(0.,0.,-1.));
#21531=DIRECTION('',(0.,0.,-1.));
#21532=DIRECTION('center_axis',(-0.500019928920193,0.866013897511261,0.));
#21533=DIRECTION('ref_axis',(-0.866013897511261,-0.500019928920193,0.));
#21534=DIRECTION('center_axis',(-0.500019928920192,-0.866013897511262,0.));
#21535=DIRECTION('ref_axis',(0.866013897511262,-0.500019928920192,0.));
#21536=DIRECTION('',(0.,0.,-1.));
#21537=DIRECTION('center_axis',(1.,0.,0.));
#21538=DIRECTION('ref_axis',(0.,0.,-1.));
#21539=DIRECTION('',(0.,0.,-1.));
#21540=DIRECTION('center_axis',(-7.25539881120531E-16,-1.,0.));
#21541=DIRECTION('ref_axis',(1.,-7.25539881120531E-16,0.));
#21542=DIRECTION('center_axis',(0.,1.,0.));
#21543=DIRECTION('ref_axis',(0.,0.,1.));
#21544=DIRECTION('',(-1.,0.,-7.03266274044652E-17));
#21545=DIRECTION('',(0.,0.,-1.));
#21546=DIRECTION('center_axis',(0.,-1.,0.));
#21547=DIRECTION('ref_axis',(0.,0.,1.));
#21548=DIRECTION('',(1.,0.,0.));
#21549=DIRECTION('',(0.,0.,1.));
#21550=DIRECTION('center_axis',(1.,0.,0.));
#21551=DIRECTION('ref_axis',(0.,0.,-1.));
#21552=DIRECTION('',(0.,-1.,0.));
#21553=DIRECTION('',(0.,0.,1.));
#21554=DIRECTION('center_axis',(-1.,0.,0.));
#21555=DIRECTION('ref_axis',(0.,0.,1.));
#21556=DIRECTION('',(0.,-1.,0.));
#21557=DIRECTION('',(0.,0.,-1.));
#21558=DIRECTION('',(0.,-1.,0.));
#21559=DIRECTION('center_axis',(0.,0.,-1.));
#21560=DIRECTION('ref_axis',(-1.,0.,0.));
#21561=DIRECTION('',(0.,-1.,0.));
#21562=DIRECTION('',(1.,0.,0.));
#21563=DIRECTION('center_axis',(0.,-1.,0.));
#21564=DIRECTION('ref_axis',(0.,0.,-1.));
#21565=DIRECTION('center_axis',(0.,-1.,0.));
#21566=DIRECTION('ref_axis',(0.,0.,-1.));
#21567=DIRECTION('center_axis',(0.,-1.,0.));
#21568=DIRECTION('ref_axis',(0.,0.,-1.));
#21569=DIRECTION('',(0.,0.,1.));
#21570=DIRECTION('',(1.,0.,7.03266274044652E-17));
#21571=DIRECTION('center_axis',(0.,1.,0.));
#21572=DIRECTION('ref_axis',(0.,0.,-1.));
#21573=DIRECTION('center_axis',(-1.,0.,0.));
#21574=DIRECTION('ref_axis',(0.,0.,1.));
#21575=DIRECTION('',(0.,0.,1.));
#21576=DIRECTION('',(0.,-1.,0.));
#21577=DIRECTION('',(0.,1.,0.));
#21578=DIRECTION('center_axis',(0.,1.,0.));
#21579=DIRECTION('ref_axis',(0.,0.,1.));
#21580=DIRECTION('center_axis',(0.,1.,0.));
#21581=DIRECTION('ref_axis',(0.,0.,-1.));
#21582=DIRECTION('center_axis',(1.,0.,7.03266274044652E-17));
#21583=DIRECTION('ref_axis',(7.03266274044652E-17,0.,-1.));
#21584=DIRECTION('center_axis',(-1.,0.,-7.03266274044652E-17));
#21585=DIRECTION('ref_axis',(7.03266274044652E-17,0.,-1.));
#21586=DIRECTION('center_axis',(-0.707106781186551,-1.56441297777777E-14,
-0.707106781186544));
#21587=DIRECTION('ref_axis',(0.707106781186544,1.21590280983195E-12,-0.707106781186551));
#21588=DIRECTION('center_axis',(0.,0.,1.));
#21589=DIRECTION('ref_axis',(1.,0.,0.));
#21590=DIRECTION('center_axis',(0.707106781186562,-4.71888504772254E-14,
-0.707106781186534));
#21591=DIRECTION('ref_axis',(0.707106781186533,-2.06008383212131E-12,0.707106781186561));
#21592=DIRECTION('center_axis',(0.,0.,1.));
#21593=DIRECTION('ref_axis',(1.,0.,0.));
#21594=DIRECTION('center_axis',(0.,0.,-1.));
#21595=DIRECTION('ref_axis',(1.,0.,0.));
#21596=DIRECTION('center_axis',(0.,0.,-1.));
#21597=DIRECTION('ref_axis',(-1.,0.,0.));
#21598=DIRECTION('center_axis',(-1.,0.,0.));
#21599=DIRECTION('ref_axis',(0.,0.,1.));
#21600=DIRECTION('center_axis',(1.,0.,0.));
#21601=DIRECTION('ref_axis',(0.,0.,-1.));
#21602=DIRECTION('center_axis',(-1.,0.,-7.03266274044652E-17));
#21603=DIRECTION('ref_axis',(-7.03266274044652E-17,0.,1.));
#21604=DIRECTION('center_axis',(-1.,0.,-7.03266274044652E-17));
#21605=DIRECTION('ref_axis',(-7.03266274044652E-17,0.,1.));
#21606=DIRECTION('center_axis',(-0.707106781186528,4.00079384480861E-14,
-0.707106781186567));
#21607=DIRECTION('ref_axis',(0.707106781186567,-1.79317795020169E-12,-0.707106781186528));
#21608=DIRECTION('center_axis',(0.,-1.,0.));
#21609=DIRECTION('ref_axis',(0.,0.,-1.));
#21610=DIRECTION('center_axis',(1.,0.,5.78241158658936E-15));
#21611=DIRECTION('ref_axis',(5.78241158658936E-15,0.,-1.));
#21612=DIRECTION('center_axis',(1.,0.,0.));
#21613=DIRECTION('ref_axis',(0.,0.,1.));
#21614=DIRECTION('center_axis',(0.,-1.,0.));
#21615=DIRECTION('ref_axis',(0.,0.,1.));
#21616=DIRECTION('center_axis',(0.,0.,1.));
#21617=DIRECTION('ref_axis',(-1.,0.,0.));
#21618=DIRECTION('center_axis',(0.,0.,-1.));
#21619=DIRECTION('ref_axis',(-1.,0.,0.));
#21620=DIRECTION('center_axis',(0.707106781186562,4.71888504772271E-14,
-0.707106781186534));
#21621=DIRECTION('ref_axis',(0.707106781186534,1.37302321411511E-12,0.707106781186561));
#21622=DIRECTION('center_axis',(0.,0.,1.));
#21623=DIRECTION('ref_axis',(1.,0.,0.));
#21624=DIRECTION('center_axis',(0.,0.,-1.));
#21625=DIRECTION('ref_axis',(1.,0.,0.));
#21626=DIRECTION('center_axis',(0.,0.,-1.));
#21627=DIRECTION('ref_axis',(-1.,0.,0.));
#21628=DIRECTION('center_axis',(1.,0.,-1.22464679914735E-16));
#21629=DIRECTION('ref_axis',(-1.22464679914735E-16,0.,-1.));
#21630=DIRECTION('center_axis',(1.,0.,0.));
#21631=DIRECTION('ref_axis',(0.,0.,-1.));
#21632=DIRECTION('center_axis',(0.,0.,-1.));
#21633=DIRECTION('ref_axis',(-1.,0.,0.));
#21634=DIRECTION('center_axis',(0.,0.,1.));
#21635=DIRECTION('ref_axis',(1.,0.,0.));
#21636=DIRECTION('center_axis',(0.,-1.,0.));
#21637=DIRECTION('ref_axis',(0.,0.,-1.));
#21638=DIRECTION('center_axis',(0.,-1.,0.));
#21639=DIRECTION('ref_axis',(0.,0.,-1.));
#21640=DIRECTION('center_axis',(1.,0.,0.));
#21641=DIRECTION('ref_axis',(0.,0.,-1.));
#21642=DIRECTION('center_axis',(1.,0.,0.));
#21643=DIRECTION('ref_axis',(0.,0.,-1.));
#21644=DIRECTION('center_axis',(0.,-1.,0.));
#21645=DIRECTION('ref_axis',(0.,0.,-1.));
#21646=DIRECTION('center_axis',(1.,0.,5.78241158658936E-15));
#21647=DIRECTION('ref_axis',(5.78241158658936E-15,0.,-1.));
#21648=DIRECTION('center_axis',(1.,0.,0.));
#21649=DIRECTION('ref_axis',(0.,0.,1.));
#21650=DIRECTION('center_axis',(0.,-1.,0.));
#21651=DIRECTION('ref_axis',(0.,0.,1.));
#21652=DIRECTION('center_axis',(1.,0.,0.));
#21653=DIRECTION('ref_axis',(0.,1.,0.));
#21654=DIRECTION('center_axis',(0.,0.,1.));
#21655=DIRECTION('ref_axis',(-1.,0.,0.));
#21656=DIRECTION('center_axis',(-1.,0.,0.));
#21657=DIRECTION('ref_axis',(0.,0.,1.));
#21658=DIRECTION('center_axis',(0.707106781186508,-4.74453116211242E-14,
0.707106781186587));
#21659=DIRECTION('ref_axis',(0.707106781186587,-1.89154275080293E-13,-0.707106781186508));
#21660=DIRECTION('center_axis',(0.,-1.,0.));
#21661=DIRECTION('ref_axis',(0.,0.,-1.));
#21662=DIRECTION('center_axis',(0.,-1.,0.));
#21663=DIRECTION('ref_axis',(0.,0.,-1.));
#21664=DIRECTION('center_axis',(0.,0.,1.));
#21665=DIRECTION('ref_axis',(1.,0.,0.));
#21666=DIRECTION('center_axis',(-1.80700362080916E-16,0.,1.));
#21667=DIRECTION('ref_axis',(1.,0.,1.80700362080916E-16));
#21668=DIRECTION('center_axis',(0.,0.,-1.));
#21669=DIRECTION('ref_axis',(-1.,0.,0.));
#21670=DIRECTION('center_axis',(0.70710678118653,-1.47892592981158E-14,
0.707106781186565));
#21671=DIRECTION('ref_axis',(0.707106781186566,-1.36695930628953E-13,-0.70710678118653));
#21672=DIRECTION('center_axis',(0.,0.,1.));
#21673=DIRECTION('ref_axis',(0.,1.,0.));
#21674=DIRECTION('center_axis',(-1.,0.,0.));
#21675=DIRECTION('ref_axis',(0.,0.,-1.));
#21676=DIRECTION('center_axis',(-1.,0.,1.22464679914735E-16));
#21677=DIRECTION('ref_axis',(1.22464679914735E-16,0.,1.));
#21678=DIRECTION('center_axis',(0.,1.,0.));
#21679=DIRECTION('ref_axis',(1.,0.,0.));
#21680=DIRECTION('center_axis',(0.,-1.,0.));
#21681=DIRECTION('ref_axis',(0.,0.,-1.));
#21682=DIRECTION('center_axis',(0.,1.,0.));
#21683=DIRECTION('ref_axis',(0.,0.,1.));
#21684=DIRECTION('center_axis',(0.707106781186578,-0.707106781186517,4.00934254960531E-14));
#21685=DIRECTION('ref_axis',(0.707106781186517,0.707106781186578,-6.1787772477201E-12));
#21686=DIRECTION('center_axis',(-1.,0.,-7.03266274044652E-17));
#21687=DIRECTION('ref_axis',(-7.03266274044652E-17,0.,1.));
#21688=DIRECTION('center_axis',(0.707106781186556,-0.707106781186539,7.35188612507565E-15));
#21689=DIRECTION('ref_axis',(0.707106781186539,0.707106781186556,-4.57157300412597E-12));
#21690=DIRECTION('center_axis',(0.,-1.,0.));
#21691=DIRECTION('ref_axis',(0.,0.,-1.));
#21692=DIRECTION('center_axis',(-0.707106781186539,-0.707106781186557,7.43737317304176E-15));
#21693=DIRECTION('ref_axis',(0.707106781186556,-0.707106781186538,-2.45750013918949E-12));
#21694=DIRECTION('center_axis',(1.,0.,7.03266274044652E-17));
#21695=DIRECTION('ref_axis',(7.03266274044652E-17,0.,-1.));
#21696=DIRECTION('center_axis',(-0.70710678118656,-0.707106781186535,-2.52186791499698E-14));
#21697=DIRECTION('ref_axis',(0.707106781186535,-0.70710678118656,-4.09319520946051E-12));
#21698=DIRECTION('center_axis',(0.,1.,0.));
#21699=DIRECTION('ref_axis',(0.,0.,1.));
#21700=DIRECTION('center_axis',(0.,-1.,0.));
#21701=DIRECTION('ref_axis',(0.,0.,-1.));
#21702=DIRECTION('center_axis',(0.,1.,0.));
#21703=DIRECTION('ref_axis',(1.,0.,0.));
#21704=DIRECTION('center_axis',(0.,0.,-1.));
#21705=DIRECTION('ref_axis',(-1.,0.,0.));
#21706=DIRECTION('center_axis',(0.,0.,-1.));
#21707=DIRECTION('ref_axis',(-1.,0.,0.));
#21708=DIRECTION('center_axis',(0.,0.,1.));
#21709=DIRECTION('ref_axis',(1.,0.,0.));
#21710=DIRECTION('center_axis',(0.,0.,1.));
#21711=DIRECTION('ref_axis',(1.,0.,0.));
#21712=DIRECTION('center_axis',(1.39659253553725E-14,-1.,-3.49148133884313E-15));
#21713=DIRECTION('ref_axis',(1.,1.1842378929335E-14,0.));
#21714=DIRECTION('center_axis',(1.39659253553725E-14,-1.,-3.49148133884313E-15));
#21715=DIRECTION('ref_axis',(1.,1.39659253553725E-14,4.71264307122384E-30));
#21716=DIRECTION('center_axis',(-5.16843062991028E-29,3.49148133884313E-15,
-1.));
#21717=DIRECTION('ref_axis',(-1.,-1.48029736616687E-14,0.));
#21718=DIRECTION('center_axis',(-1.39659253553725E-14,1.,3.49148133884313E-15));
#21719=DIRECTION('ref_axis',(1.,1.39659253553726E-14,-1.73472347597681E-14));
#21720=DIRECTION('center_axis',(-1.39659253553725E-14,1.,3.49148133884313E-15));
#21721=DIRECTION('ref_axis',(1.,1.39659253553726E-14,-1.73472347597681E-14));
#21722=DIRECTION('center_axis',(1.39659253553725E-14,-1.,-3.49148133884313E-15));
#21723=DIRECTION('ref_axis',(1.,1.1842378929335E-14,0.));
#21724=DIRECTION('center_axis',(1.39659253553725E-14,-1.,-3.49148133884313E-15));
#21725=DIRECTION('ref_axis',(1.,1.39659253553725E-14,8.38340346178524E-30));
#21726=DIRECTION('center_axis',(1.39659253553725E-14,-1.,-3.49148133884313E-15));
#21727=DIRECTION('ref_axis',(1.,1.39659253553725E-14,8.38340346178524E-30));
#21728=DIRECTION('center_axis',(-5.16843062991028E-29,3.49148133884313E-15,
-1.));
#21729=DIRECTION('ref_axis',(-1.,-1.48029736616687E-14,0.));
#21730=DIRECTION('center_axis',(-1.39659253553725E-14,1.,3.49148133884313E-15));
#21731=DIRECTION('ref_axis',(1.,1.39659253553725E-14,4.71264307122384E-30));
#21732=DIRECTION('center_axis',(-1.39659253553725E-14,1.,3.49148133884313E-15));
#21733=DIRECTION('ref_axis',(-1.,-1.39659253553725E-14,-8.38340346178524E-30));
#21734=DIRECTION('',(1.39659253553725E-14,-1.,-3.49148133884313E-15));
#21735=DIRECTION('center_axis',(1.39659253553725E-14,-1.,-3.49148133884313E-15));
#21736=DIRECTION('ref_axis',(1.,1.39659253553725E-14,4.87617677579594E-29));
#21737=DIRECTION('center_axis',(1.39659253553725E-14,-1.,-3.49148133884313E-15));
#21738=DIRECTION('ref_axis',(1.,1.39659253553725E-14,4.87617677579594E-29));
#21739=DIRECTION('center_axis',(-0.999752444790186,-3.23231498703571E-17,
-0.0222496996844003));
#21740=DIRECTION('ref_axis',(-3.23151481062091E-17,1.,-7.19180377469308E-19));
#21741=DIRECTION('center_axis',(0.999752444790186,3.23231498703571E-17,
0.0222496996844003));
#21742=DIRECTION('ref_axis',(3.23151481062091E-17,-1.,7.19180377469308E-19));
#21743=DIRECTION('',(0.999752444790186,3.23231498703571E-17,0.0222496996844003));
#21744=DIRECTION('center_axis',(0.999752444790186,3.23231498703571E-17,
0.0222496996844003));
#21745=DIRECTION('ref_axis',(3.23151481062091E-17,-1.,7.19180377469308E-19));
#21746=DIRECTION('center_axis',(-0.999752444790186,-3.23231498703571E-17,
-0.0222496996844003));
#21747=DIRECTION('ref_axis',(-3.23151481062091E-17,1.,-7.19180377469308E-19));
#21748=DIRECTION('center_axis',(0.999752444790186,3.23231498703571E-17,
0.0222496996844003));
#21749=DIRECTION('ref_axis',(3.23151481062091E-17,-1.,7.19180377469308E-19));
#21750=DIRECTION('center_axis',(0.999752444790186,3.23231498703571E-17,
0.0222496996844003));
#21751=DIRECTION('ref_axis',(3.23151481062091E-17,-1.,7.19180377469308E-19));
#21752=DIRECTION('',(0.999752444790186,3.23231498703571E-17,0.0222496996844003));
#21753=DIRECTION('center_axis',(0.999752444790186,3.23231498703571E-17,
0.0222496996844003));
#21754=DIRECTION('ref_axis',(3.23151481062091E-17,-1.,7.19180377469308E-19));
#21755=DIRECTION('center_axis',(0.999752444790186,3.23231498703571E-17,
0.0222496996844003));
#21756=DIRECTION('ref_axis',(3.23151481062091E-17,-1.,7.19180377469308E-19));
#21757=DIRECTION('center_axis',(-0.0222496996844003,-1.18122020847398E-16,
0.999752444790186));
#21758=DIRECTION('ref_axis',(0.999752444790186,4.16004662851392E-32,0.0222496996844003));
#21759=DIRECTION('center_axis',(-0.0222496996844003,-1.18122020847398E-16,
0.999752444790186));
#21760=DIRECTION('ref_axis',(0.999752444790186,4.16004662851392E-32,0.0222496996844003));
#21761=DIRECTION('',(-0.0222496996844003,-1.18122020847398E-16,0.999752444790186));
#21762=DIRECTION('center_axis',(-0.0222496996844003,-1.18122020847398E-16,
0.999752444790186));
#21763=DIRECTION('ref_axis',(0.999752444790186,4.16004662851392E-32,0.0222496996844003));
#21764=DIRECTION('center_axis',(3.49433275961782E-17,-1.,-1.17373598748275E-16));
#21765=DIRECTION('ref_axis',(-0.999752444790186,-3.23231498703574E-17,-0.0222496996843981));
#21766=DIRECTION('center_axis',(3.49433275961782E-17,-1.,-1.17373598748275E-16));
#21767=DIRECTION('ref_axis',(-0.999752444790186,-3.23231498703574E-17,-0.0222496996843981));
#21768=DIRECTION('',(3.49433275961782E-17,-1.,-1.17373598748275E-16));
#21769=DIRECTION('center_axis',(-3.49433275961782E-17,1.,1.17373598748275E-16));
#21770=DIRECTION('ref_axis',(0.999752444790186,3.23231498703574E-17,0.0222496996843981));
#21771=DIRECTION('center_axis',(3.49433275961782E-17,-1.,-1.17373598748275E-16));
#21772=DIRECTION('ref_axis',(-0.999752444790186,-3.23231498703574E-17,-0.0222496996843981));
#21773=DIRECTION('center_axis',(-3.49433275961782E-17,1.,1.17373598748275E-16));
#21774=DIRECTION('ref_axis',(0.999752444790186,3.23231498703574E-17,0.0222496996843981));
#21775=DIRECTION('',(3.49433275961782E-17,-1.,-1.17373598748275E-16));
#21776=DIRECTION('center_axis',(-3.49433275961782E-17,1.,1.17373598748275E-16));
#21777=DIRECTION('ref_axis',(0.999752444790186,3.23231498703574E-17,0.0222496996843981));
#21778=DIRECTION('center_axis',(-0.0222496996844003,-1.18122020847398E-16,
0.999752444790186));
#21779=DIRECTION('ref_axis',(0.999752444790186,-1.2958542423238E-31,0.0222496996844003));
#21780=DIRECTION('center_axis',(-0.0222496996844003,-1.18122020847398E-16,
0.999752444790186));
#21781=DIRECTION('ref_axis',(0.999752444790186,-1.2958542423238E-31,0.0222496996844003));
#21782=DIRECTION('',(-0.0222496996844003,-1.18122020847398E-16,0.999752444790186));
#21783=DIRECTION('center_axis',(0.0222496996844003,1.18122020847398E-16,
-0.999752444790186));
#21784=DIRECTION('ref_axis',(0.999752444790186,-1.2958542423238E-31,0.0222496996844003));
#21785=DIRECTION('center_axis',(-0.999752444790186,-3.23231498703571E-17,
-0.0222496996844003));
#21786=DIRECTION('ref_axis',(-3.49433275961782E-17,1.,1.17373598748275E-16));
#21787=DIRECTION('',(3.49433275961782E-17,-1.,-1.17373598748275E-16));
#21788=DIRECTION('',(0.0222496996844003,1.18122020847398E-16,-0.999752444790186));
#21789=DIRECTION('',(3.49433275961782E-17,-1.,-1.17373598748275E-16));
#21790=DIRECTION('center_axis',(3.49433275961782E-17,-1.,-1.17373598748275E-16));
#21791=DIRECTION('ref_axis',(-0.999752444790186,-3.23231498703571E-17,-0.0222496996844003));
#21792=DIRECTION('',(3.49433275961782E-17,-1.,-1.17373598748275E-16));
#21793=DIRECTION('center_axis',(-3.49433275961782E-17,1.,1.17373598748275E-16));
#21794=DIRECTION('ref_axis',(0.999752444790186,3.23231498703571E-17,0.0222496996844003));
#21795=DIRECTION('',(3.49433275961782E-17,-1.,-1.17373598748275E-16));
#21796=DIRECTION('center_axis',(-3.49433275961782E-17,1.,1.17373598748275E-16));
#21797=DIRECTION('ref_axis',(-0.999752444790186,-3.23231498703571E-17,-0.0222496996844003));
#21798=DIRECTION('center_axis',(0.999752444790186,3.23231498703571E-17,
0.0222496996844003));
#21799=DIRECTION('ref_axis',(3.49433275961782E-17,-1.,-1.17373598748275E-16));
#21800=DIRECTION('',(-0.0222496996844003,-1.18122020847398E-16,0.999752444790186));
#21801=DIRECTION('',(3.49433275961782E-17,-1.,-1.17373598748275E-16));
#21802=DIRECTION('',(-0.0222496996844003,-1.18122020847398E-16,0.999752444790186));
#21803=DIRECTION('center_axis',(3.49433275961782E-17,-1.,-1.17373598748275E-16));
#21804=DIRECTION('ref_axis',(-0.999752444790186,-3.23231498703571E-17,-0.0222496996844003));
#21805=DIRECTION('',(-0.999752444790186,-3.23231498703571E-17,-0.0222496996844003));
#21806=DIRECTION('',(0.999752444790186,3.23231498703571E-17,0.0222496996844003));
#21807=DIRECTION('center_axis',(3.49433275961782E-17,-1.,-1.17373598748275E-16));
#21808=DIRECTION('ref_axis',(-0.999752444790186,-3.23231498703571E-17,-0.0222496996844003));
#21809=DIRECTION('',(0.0222496996844003,1.18122020847398E-16,-0.999752444790186));
#21810=DIRECTION('',(0.999752444790186,3.23231498703571E-17,0.0222496996844003));
#21811=DIRECTION('',(-0.0222496996844003,-1.18122020847398E-16,0.999752444790186));
#21812=DIRECTION('center_axis',(-3.49433275961782E-17,1.,1.17373598748275E-16));
#21813=DIRECTION('ref_axis',(-0.999752444790186,-3.23231498703571E-17,-0.0222496996844003));
#21814=DIRECTION('',(-0.999752444790186,-3.23231498703571E-17,-0.0222496996844003));
#21815=DIRECTION('center_axis',(-0.999752444790186,-3.23231498703571E-17,
-0.0222496996844003));
#21816=DIRECTION('ref_axis',(-3.49433275961782E-17,1.,1.17373598748275E-16));
#21817=DIRECTION('',(3.49433275961782E-17,-1.,-1.17373598748275E-16));
#21818=DIRECTION('',(3.49433275961782E-17,-1.,-1.17373598748275E-16));
#21819=DIRECTION('center_axis',(-0.0222496996844003,-1.18122020847398E-16,
0.999752444790186));
#21820=DIRECTION('ref_axis',(0.999752444790186,3.23231498703571E-17,0.0222496996844003));
#21821=DIRECTION('',(3.49433275961782E-17,-1.,-1.17373598748275E-16));
#21822=DIRECTION('',(0.999752444790186,3.23231498703571E-17,0.0222496996844003));
#21823=DIRECTION('',(3.49433275961782E-17,-1.,-1.17373598748275E-16));
#21824=DIRECTION('',(-0.999752444790186,-3.23231498703571E-17,-0.0222496996844003));
#21825=DIRECTION('center_axis',(3.49433275961782E-17,-1.,-1.17373598748275E-16));
#21826=DIRECTION('ref_axis',(-0.999752444790186,-3.23231498703571E-17,-0.0222496996844003));
#21827=DIRECTION('',(3.49433275961782E-17,-1.,-1.17373598748275E-16));
#21828=DIRECTION('center_axis',(3.49433275961782E-17,-1.,-1.17373598748275E-16));
#21829=DIRECTION('ref_axis',(-0.999752444790186,-3.23231498703571E-17,-0.0222496996844003));
#21830=DIRECTION('center_axis',(0.999752444790186,3.23231498703571E-17,
0.0222496996844003));
#21831=DIRECTION('ref_axis',(3.49433275961782E-17,-1.,-1.17373598748275E-16));
#21832=DIRECTION('',(3.49433275961782E-17,-1.,-1.17373598748275E-16));
#21833=DIRECTION('',(0.0222496996844003,1.18122020847398E-16,-0.999752444790186));
#21834=DIRECTION('center_axis',(0.0222496996844003,1.18122020847398E-16,
-0.999752444790186));
#21835=DIRECTION('ref_axis',(-0.999752444790186,-3.23231498703571E-17,-0.0222496996844003));
#21836=DIRECTION('',(0.999752444790186,3.23231498703571E-17,0.0222496996844003));
#21837=DIRECTION('',(3.49433275961782E-17,-1.,-1.17373598748275E-16));
#21838=DIRECTION('',(-0.999752444790186,-3.23231498703571E-17,-0.0222496996844003));
#21839=DIRECTION('center_axis',(-3.49433275961782E-17,1.,1.17373598748275E-16));
#21840=DIRECTION('ref_axis',(0.999752444790186,3.23231498703571E-17,0.0222496996844003));
#21841=DIRECTION('',(0.0222496996844003,1.18122020847398E-16,-0.999752444790186));
#21842=DIRECTION('center_axis',(3.49433275961782E-17,-1.,-1.17373598748275E-16));
#21843=DIRECTION('ref_axis',(-0.999752444790186,-3.23231498703571E-17,-0.0222496996844003));
#21844=DIRECTION('',(0.0222496996844003,1.18122020847398E-16,-0.999752444790186));
#21845=DIRECTION('center_axis',(0.999752444790186,3.23231498703571E-17,
0.0222496996844003));
#21846=DIRECTION('ref_axis',(0.0222496996844003,1.18122020847398E-16,-0.999752444790186));
#21847=DIRECTION('center_axis',(-0.0222496996844003,-1.18122020847398E-16,
0.999752444790186));
#21848=DIRECTION('ref_axis',(0.999752444790186,3.23231498703571E-17,0.0222496996844003));
#21849=DIRECTION('center_axis',(0.999752444790186,3.23231498703571E-17,
0.0222496996844003));
#21850=DIRECTION('ref_axis',(3.49433275961782E-17,-1.,-1.17373598748275E-16));
#21851=DIRECTION('center_axis',(0.999752444790186,3.23231498703571E-17,
0.0222496996844003));
#21852=DIRECTION('ref_axis',(3.49433275961782E-17,-1.,-1.17373598748275E-16));
#21853=DIRECTION('center_axis',(0.999752444790186,6.00249380122153E-17,
0.0222496996843998));
#21854=DIRECTION('ref_axis',(-0.0220459940098395,-0.135007583468649,0.990599276475646));
#21855=DIRECTION('center_axis',(0.999752444790186,6.00249380122153E-17,
0.0222496996843998));
#21856=DIRECTION('ref_axis',(-0.0220459940098395,-0.135007583468649,0.990599276475646));
#21857=DIRECTION('',(0.999752444790186,6.00249380122153E-17,0.0222496996843998));
#21858=DIRECTION('center_axis',(0.999752444790186,6.00249380122153E-17,
0.0222496996843998));
#21859=DIRECTION('ref_axis',(-0.0220459940098395,-0.135007583468649,0.990599276475646));
#21860=DIRECTION('center_axis',(-0.00300387818729384,0.99084456520988,0.134974161637996));
#21861=DIRECTION('ref_axis',(0.0220459940098398,0.135007583468648,-0.990599276475646));
#21862=DIRECTION('center_axis',(0.999752444790186,1.11968515267594E-16,
0.0222496996843994));
#21863=DIRECTION('ref_axis',(-0.0220459940098391,-0.135007583468648,0.990599276475646));
#21864=DIRECTION('center_axis',(-0.999752444790186,-5.98479599211999E-17,
-0.0222496996843998));
#21865=DIRECTION('ref_axis',(0.0220459940098395,0.135007583468649,-0.990599276475646));
#21866=DIRECTION('center_axis',(-2.44929359829471E-16,0.,-1.));
#21867=DIRECTION('ref_axis',(-1.,0.,0.));
#21868=DIRECTION('center_axis',(-2.44929359829471E-16,0.,-1.));
#21869=DIRECTION('ref_axis',(-1.,0.,2.44929359829471E-16));
#21870=DIRECTION('center_axis',(0.,1.,0.));
#21871=DIRECTION('ref_axis',(1.,0.,0.));
#21872=DIRECTION('center_axis',(2.44929359829471E-16,0.,1.));
#21873=DIRECTION('ref_axis',(-1.,0.,2.44929359829471E-16));
#21874=DIRECTION('center_axis',(-2.44929359829471E-16,0.,-1.));
#21875=DIRECTION('ref_axis',(-1.,0.,2.44929359829471E-16));
#21876=DIRECTION('center_axis',(-2.44929359829471E-16,-1.22460635382238E-16,
-1.));
#21877=DIRECTION('ref_axis',(-2.99942050284817E-32,1.,-1.22460635382238E-16));
#21878=DIRECTION('center_axis',(-2.44929359829471E-16,-1.22460635382238E-16,
-1.));
#21879=DIRECTION('ref_axis',(-2.99942050284817E-32,1.,-1.22460635382238E-16));
#21880=DIRECTION('',(-0.707106781186546,8.65956056235492E-17,0.707106781186549));
#21881=DIRECTION('center_axis',(-2.44929359829471E-16,0.,-1.));
#21882=DIRECTION('ref_axis',(-1.,0.,2.44929359829471E-16));
#21883=DIRECTION('center_axis',(-2.44929359829471E-16,-1.22460635382238E-16,
-1.));
#21884=DIRECTION('ref_axis',(2.99942050284817E-32,-1.,1.22460635382238E-16));
#21885=DIRECTION('center_axis',(-2.44929359829471E-16,-1.22460635382238E-16,
-1.));
#21886=DIRECTION('ref_axis',(2.99942050284817E-32,-1.,1.22460635382238E-16));
#21887=DIRECTION('center_axis',(-2.44929359829471E-16,-1.22460635382238E-16,
-1.));
#21888=DIRECTION('ref_axis',(2.99942050284817E-32,-1.,1.22460635382238E-16));
#21889=DIRECTION('',(4.01685164633802E-17,-0.819152044288988,0.573576436351052));
#21890=DIRECTION('center_axis',(-2.44929359829471E-16,-1.22460635382238E-16,
-1.));
#21891=DIRECTION('ref_axis',(2.99942050284817E-32,-1.,1.22460635382238E-16));
#21892=DIRECTION('center_axis',(-2.44929359829471E-16,-1.22460635382238E-16,
-1.));
#21893=DIRECTION('ref_axis',(2.99942050284817E-32,-1.,1.22460635382238E-16));
#21894=DIRECTION('center_axis',(2.44929359829471E-16,1.22460635382238E-16,
1.));
#21895=DIRECTION('ref_axis',(-2.99942050284817E-32,1.,-1.22460635382238E-16));
#21896=DIRECTION('',(-2.40802902274083E-16,0.819152044288993,-0.573576436351044));
#21897=DIRECTION('center_axis',(-2.44929359829471E-16,0.,-1.));
#21898=DIRECTION('ref_axis',(-1.,0.,2.44929359829471E-16));
#21899=DIRECTION('center_axis',(-2.44929359829471E-16,-1.22460635382238E-16,
-1.));
#21900=DIRECTION('ref_axis',(2.99942050284817E-32,-1.,1.22460635382238E-16));
#21901=DIRECTION('center_axis',(-2.44929359829471E-16,-1.22460635382238E-16,
-1.));
#21902=DIRECTION('ref_axis',(2.99942050284817E-32,-1.,1.22460635382238E-16));
#21903=DIRECTION('',(2.44929359829471E-16,0.,1.));
#21904=DIRECTION('center_axis',(-2.44929359829471E-16,-1.22460635382238E-16,
-1.));
#21905=DIRECTION('ref_axis',(2.99942050284817E-32,-1.,1.22460635382238E-16));
#21906=DIRECTION('center_axis',(-2.44929359829471E-16,-1.22460635382238E-16,
-1.));
#21907=DIRECTION('ref_axis',(2.99942050284817E-32,-1.,1.22460635382238E-16));
#21908=DIRECTION('center_axis',(-2.44929359829471E-16,-1.22460635382238E-16,
-1.));
#21909=DIRECTION('ref_axis',(2.99942050284817E-32,-1.,1.22460635382238E-16));
#21910=DIRECTION('',(4.01685164633802E-17,-0.819152044288988,0.573576436351052));
#21911=DIRECTION('center_axis',(-2.44929359829471E-16,-1.22460635382238E-16,
-1.));
#21912=DIRECTION('ref_axis',(2.99942050284817E-32,-1.,1.22460635382238E-16));
#21913=DIRECTION('center_axis',(-2.44929359829471E-16,-1.22460635382238E-16,
-1.));
#21914=DIRECTION('ref_axis',(2.99942050284817E-32,-1.,1.22460635382238E-16));
#21915=DIRECTION('center_axis',(2.44929359829471E-16,1.22460635382238E-16,
1.));
#21916=DIRECTION('ref_axis',(-2.99942050284817E-32,1.,-1.22460635382238E-16));
#21917=DIRECTION('',(-2.40802902274083E-16,0.819152044288993,-0.573576436351044));
#21918=DIRECTION('center_axis',(-2.44929359829471E-16,0.,-1.));
#21919=DIRECTION('ref_axis',(-1.,0.,2.44929359829471E-16));
#21920=DIRECTION('center_axis',(-2.44929359829471E-16,-1.22460635382238E-16,
-1.));
#21921=DIRECTION('ref_axis',(2.99942050284817E-32,-1.,1.22460635382238E-16));
#21922=DIRECTION('center_axis',(-2.44929359829471E-16,-1.22460635382238E-16,
-1.));
#21923=DIRECTION('ref_axis',(2.99942050284817E-32,-1.,1.22460635382238E-16));
#21924=DIRECTION('',(2.44929359829471E-16,0.,1.));
#21925=DIRECTION('center_axis',(-2.44929359829471E-16,-1.22460635382238E-16,
-1.));
#21926=DIRECTION('ref_axis',(2.99942050284817E-32,-1.,1.22460635382238E-16));
#21927=DIRECTION('center_axis',(-2.44929359829471E-16,-1.22460635382238E-16,
-1.));
#21928=DIRECTION('ref_axis',(2.99942050284817E-32,-1.,1.22460635382238E-16));
#21929=DIRECTION('center_axis',(-2.44929359829471E-16,-1.22460635382238E-16,
-1.));
#21930=DIRECTION('ref_axis',(2.99942050284817E-32,-1.,1.22460635382238E-16));
#21931=DIRECTION('',(4.01685164633802E-17,-0.819152044288988,0.573576436351052));
#21932=DIRECTION('center_axis',(-2.44929359829471E-16,-1.22460635382238E-16,
-1.));
#21933=DIRECTION('ref_axis',(2.99942050284817E-32,-1.,1.22460635382238E-16));
#21934=DIRECTION('center_axis',(-2.44929359829471E-16,-1.22460635382238E-16,
-1.));
#21935=DIRECTION('ref_axis',(2.99942050284817E-32,-1.,1.22460635382238E-16));
#21936=DIRECTION('center_axis',(2.44929359829471E-16,1.22460635382238E-16,
1.));
#21937=DIRECTION('ref_axis',(-2.99942050284817E-32,1.,-1.22460635382238E-16));
#21938=DIRECTION('',(-2.40802902274083E-16,0.819152044288993,-0.573576436351044));
#21939=DIRECTION('center_axis',(-2.44929359829471E-16,0.,-1.));
#21940=DIRECTION('ref_axis',(-1.,0.,2.44929359829471E-16));
#21941=DIRECTION('center_axis',(-2.44929359829471E-16,-1.22460635382238E-16,
-1.));
#21942=DIRECTION('ref_axis',(2.99942050284817E-32,-1.,1.22460635382238E-16));
#21943=DIRECTION('center_axis',(-2.44929359829471E-16,-1.22460635382238E-16,
-1.));
#21944=DIRECTION('ref_axis',(2.99942050284817E-32,-1.,1.22460635382238E-16));
#21945=DIRECTION('',(2.44929359829471E-16,0.,1.));
#21946=DIRECTION('center_axis',(-2.44929359829471E-16,-1.22460635382238E-16,
-1.));
#21947=DIRECTION('ref_axis',(2.99942050284817E-32,-1.,1.22460635382238E-16));
#21948=DIRECTION('center_axis',(-2.44929359829471E-16,-1.22460635382238E-16,
-1.));
#21949=DIRECTION('ref_axis',(2.99942050284817E-32,-1.,1.22460635382238E-16));
#21950=DIRECTION('center_axis',(-2.44929359829471E-16,-1.22460635382238E-16,
-1.));
#21951=DIRECTION('ref_axis',(2.99942050284817E-32,-1.,1.22460635382238E-16));
#21952=DIRECTION('',(4.01685164633802E-17,-0.819152044288988,0.573576436351052));
#21953=DIRECTION('center_axis',(-2.44929359829471E-16,-1.22460635382238E-16,
-1.));
#21954=DIRECTION('ref_axis',(2.99942050284817E-32,-1.,1.22460635382238E-16));
#21955=DIRECTION('center_axis',(-2.44929359829471E-16,-1.22460635382238E-16,
-1.));
#21956=DIRECTION('ref_axis',(2.99942050284817E-32,-1.,1.22460635382238E-16));
#21957=DIRECTION('center_axis',(2.44929359829471E-16,1.22460635382238E-16,
1.));
#21958=DIRECTION('ref_axis',(-2.99942050284817E-32,1.,-1.22460635382238E-16));
#21959=DIRECTION('',(-2.40802902274083E-16,0.819152044288993,-0.573576436351044));
#21960=DIRECTION('center_axis',(-2.44929359829471E-16,0.,-1.));
#21961=DIRECTION('ref_axis',(-1.,0.,2.44929359829471E-16));
#21962=DIRECTION('center_axis',(-2.44929359829471E-16,-1.22460635382238E-16,
-1.));
#21963=DIRECTION('ref_axis',(2.99942050284817E-32,-1.,1.22460635382238E-16));
#21964=DIRECTION('center_axis',(-2.44929359829471E-16,-1.22460635382238E-16,
-1.));
#21965=DIRECTION('ref_axis',(2.99942050284817E-32,-1.,1.22460635382238E-16));
#21966=DIRECTION('',(2.44929359829471E-16,0.,1.));
#21967=DIRECTION('center_axis',(-2.44929359829471E-16,-1.22460635382238E-16,
-1.));
#21968=DIRECTION('ref_axis',(2.99942050284817E-32,-1.,1.22460635382238E-16));
#21969=DIRECTION('center_axis',(-2.44929359829471E-16,-1.22460635382238E-16,
-1.));
#21970=DIRECTION('ref_axis',(2.99942050284817E-32,-1.,1.22460635382238E-16));
#21971=DIRECTION('center_axis',(-2.44929359829471E-16,-1.22460635382238E-16,
-1.));
#21972=DIRECTION('ref_axis',(2.99942050284817E-32,-1.,1.22460635382238E-16));
#21973=DIRECTION('',(4.01685164633802E-17,-0.819152044288988,0.573576436351052));
#21974=DIRECTION('center_axis',(-2.44929359829471E-16,-1.22460635382238E-16,
-1.));
#21975=DIRECTION('ref_axis',(2.99942050284817E-32,-1.,1.22460635382238E-16));
#21976=DIRECTION('center_axis',(-2.44929359829471E-16,-1.22460635382238E-16,
-1.));
#21977=DIRECTION('ref_axis',(2.99942050284817E-32,-1.,1.22460635382238E-16));
#21978=DIRECTION('center_axis',(2.44929359829471E-16,1.22460635382238E-16,
1.));
#21979=DIRECTION('ref_axis',(-2.99942050284817E-32,1.,-1.22460635382238E-16));
#21980=DIRECTION('',(-2.40802902274083E-16,0.819152044288993,-0.573576436351044));
#21981=DIRECTION('center_axis',(-2.44929359829471E-16,0.,-1.));
#21982=DIRECTION('ref_axis',(-1.,0.,2.44929359829471E-16));
#21983=DIRECTION('center_axis',(-2.44929359829471E-16,-1.22460635382238E-16,
-1.));
#21984=DIRECTION('ref_axis',(2.99942050284817E-32,-1.,1.22460635382238E-16));
#21985=DIRECTION('center_axis',(-2.44929359829471E-16,-1.22460635382238E-16,
-1.));
#21986=DIRECTION('ref_axis',(2.99942050284817E-32,-1.,1.22460635382238E-16));
#21987=DIRECTION('',(2.44929359829471E-16,0.,1.));
#21988=DIRECTION('center_axis',(-2.44929359829471E-16,-1.22460635382238E-16,
-1.));
#21989=DIRECTION('ref_axis',(2.99942050284817E-32,-1.,1.22460635382238E-16));
#21990=DIRECTION('center_axis',(-2.44929359829471E-16,-1.22460635382238E-16,
-1.));
#21991=DIRECTION('ref_axis',(2.99942050284817E-32,-1.,1.22460635382238E-16));
#21992=DIRECTION('center_axis',(-2.44929359829471E-16,-1.22460635382238E-16,
-1.));
#21993=DIRECTION('ref_axis',(2.99942050284817E-32,-1.,1.22460635382238E-16));
#21994=DIRECTION('',(4.01685164633802E-17,-0.819152044288988,0.573576436351052));
#21995=DIRECTION('center_axis',(-2.44929359829471E-16,-1.22460635382238E-16,
-1.));
#21996=DIRECTION('ref_axis',(2.99942050284817E-32,-1.,1.22460635382238E-16));
#21997=DIRECTION('center_axis',(-2.44929359829471E-16,-1.22460635382238E-16,
-1.));
#21998=DIRECTION('ref_axis',(2.99942050284817E-32,-1.,1.22460635382238E-16));
#21999=DIRECTION('center_axis',(2.44929359829471E-16,1.22460635382238E-16,
1.));
#22000=DIRECTION('ref_axis',(-2.99942050284817E-32,1.,-1.22460635382238E-16));
#22001=DIRECTION('',(-2.40802902274083E-16,0.819152044288993,-0.573576436351044));
#22002=DIRECTION('center_axis',(-2.44929359829471E-16,0.,-1.));
#22003=DIRECTION('ref_axis',(-1.,0.,2.44929359829471E-16));
#22004=DIRECTION('center_axis',(-2.44929359829471E-16,-1.22460635382238E-16,
-1.));
#22005=DIRECTION('ref_axis',(2.99942050284817E-32,-1.,1.22460635382238E-16));
#22006=DIRECTION('center_axis',(-2.44929359829471E-16,-1.22460635382238E-16,
-1.));
#22007=DIRECTION('ref_axis',(2.99942050284817E-32,-1.,1.22460635382238E-16));
#22008=DIRECTION('',(2.44929359829471E-16,0.,1.));
#22009=DIRECTION('center_axis',(-2.44929359829471E-16,-1.22460635382238E-16,
-1.));
#22010=DIRECTION('ref_axis',(2.99942050284817E-32,-1.,1.22460635382238E-16));
#22011=DIRECTION('center_axis',(-2.44929359829471E-16,-1.22460635382238E-16,
-1.));
#22012=DIRECTION('ref_axis',(2.99942050284817E-32,-1.,1.22460635382238E-16));
#22013=DIRECTION('center_axis',(-2.44929359829471E-16,-1.22460635382238E-16,
-1.));
#22014=DIRECTION('ref_axis',(2.99942050284817E-32,-1.,1.22460635382238E-16));
#22015=DIRECTION('',(4.01685164633802E-17,-0.819152044288988,0.573576436351052));
#22016=DIRECTION('center_axis',(-2.44929359829471E-16,-1.22460635382238E-16,
-1.));
#22017=DIRECTION('ref_axis',(2.99942050284817E-32,-1.,1.22460635382238E-16));
#22018=DIRECTION('center_axis',(-2.44929359829471E-16,-1.22460635382238E-16,
-1.));
#22019=DIRECTION('ref_axis',(2.99942050284817E-32,-1.,1.22460635382238E-16));
#22020=DIRECTION('center_axis',(2.44929359829471E-16,1.22460635382238E-16,
1.));
#22021=DIRECTION('ref_axis',(-2.99942050284817E-32,1.,-1.22460635382238E-16));
#22022=DIRECTION('',(-2.40802902274083E-16,0.819152044288993,-0.573576436351044));
#22023=DIRECTION('center_axis',(-2.44929359829471E-16,0.,-1.));
#22024=DIRECTION('ref_axis',(-1.,0.,2.44929359829471E-16));
#22025=DIRECTION('center_axis',(-2.44929359829471E-16,-1.22460635382238E-16,
-1.));
#22026=DIRECTION('ref_axis',(2.99942050284817E-32,-1.,1.22460635382238E-16));
#22027=DIRECTION('center_axis',(-2.44929359829471E-16,-1.22460635382238E-16,
-1.));
#22028=DIRECTION('ref_axis',(2.99942050284817E-32,-1.,1.22460635382238E-16));
#22029=DIRECTION('',(2.44929359829471E-16,0.,1.));
#22030=DIRECTION('center_axis',(-2.44929359829471E-16,-1.22460635382238E-16,
-1.));
#22031=DIRECTION('ref_axis',(2.99942050284817E-32,-1.,1.22460635382238E-16));
#22032=DIRECTION('center_axis',(-2.44929359829471E-16,-1.22460635382238E-16,
-1.));
#22033=DIRECTION('ref_axis',(2.99942050284817E-32,-1.,1.22460635382238E-16));
#22034=DIRECTION('center_axis',(-2.44929359829471E-16,-1.22460635382238E-16,
-1.));
#22035=DIRECTION('ref_axis',(2.99942050284817E-32,-1.,1.22460635382238E-16));
#22036=DIRECTION('',(4.01685164633802E-17,-0.819152044288988,0.573576436351052));
#22037=DIRECTION('center_axis',(-2.44929359829471E-16,-1.22460635382238E-16,
-1.));
#22038=DIRECTION('ref_axis',(2.99942050284817E-32,-1.,1.22460635382238E-16));
#22039=DIRECTION('center_axis',(-2.44929359829471E-16,-1.22460635382238E-16,
-1.));
#22040=DIRECTION('ref_axis',(2.99942050284817E-32,-1.,1.22460635382238E-16));
#22041=DIRECTION('center_axis',(2.44929359829471E-16,1.22460635382238E-16,
1.));
#22042=DIRECTION('ref_axis',(-2.99942050284817E-32,1.,-1.22460635382238E-16));
#22043=DIRECTION('',(-2.40802902274083E-16,0.819152044288993,-0.573576436351044));
#22044=DIRECTION('center_axis',(-2.44929359829471E-16,0.,-1.));
#22045=DIRECTION('ref_axis',(-1.,0.,2.44929359829471E-16));
#22046=DIRECTION('center_axis',(-2.44929359829471E-16,-1.22460635382238E-16,
-1.));
#22047=DIRECTION('ref_axis',(2.99942050284817E-32,-1.,1.22460635382238E-16));
#22048=DIRECTION('center_axis',(-2.44929359829471E-16,-1.22460635382238E-16,
-1.));
#22049=DIRECTION('ref_axis',(2.99942050284817E-32,-1.,1.22460635382238E-16));
#22050=DIRECTION('',(2.44929359829471E-16,0.,1.));
#22051=DIRECTION('center_axis',(-2.44929359829471E-16,-1.22460635382238E-16,
-1.));
#22052=DIRECTION('ref_axis',(2.99942050284817E-32,-1.,1.22460635382238E-16));
#22053=DIRECTION('center_axis',(-2.44929359829471E-16,-1.22460635382238E-16,
-1.));
#22054=DIRECTION('ref_axis',(2.99942050284817E-32,-1.,1.22460635382238E-16));
#22055=DIRECTION('center_axis',(-2.44929359829471E-16,-1.22460635382238E-16,
-1.));
#22056=DIRECTION('ref_axis',(2.99942050284817E-32,-1.,1.22460635382238E-16));
#22057=DIRECTION('',(4.01685164633802E-17,-0.819152044288988,0.573576436351052));
#22058=DIRECTION('center_axis',(-2.44929359829471E-16,-1.22460635382238E-16,
-1.));
#22059=DIRECTION('ref_axis',(2.99942050284817E-32,-1.,1.22460635382238E-16));
#22060=DIRECTION('center_axis',(-2.44929359829471E-16,-1.22460635382238E-16,
-1.));
#22061=DIRECTION('ref_axis',(2.99942050284817E-32,-1.,1.22460635382238E-16));
#22062=DIRECTION('center_axis',(2.44929359829471E-16,1.22460635382238E-16,
1.));
#22063=DIRECTION('ref_axis',(-2.99942050284817E-32,1.,-1.22460635382238E-16));
#22064=DIRECTION('',(-2.40802902274083E-16,0.819152044288993,-0.573576436351044));
#22065=DIRECTION('center_axis',(-2.44929359829471E-16,0.,-1.));
#22066=DIRECTION('ref_axis',(-1.,0.,2.44929359829471E-16));
#22067=DIRECTION('center_axis',(-2.44929359829471E-16,-1.22460635382238E-16,
-1.));
#22068=DIRECTION('ref_axis',(2.99942050284817E-32,-1.,1.22460635382238E-16));
#22069=DIRECTION('center_axis',(-2.44929359829471E-16,-1.22460635382238E-16,
-1.));
#22070=DIRECTION('ref_axis',(2.99942050284817E-32,-1.,1.22460635382238E-16));
#22071=DIRECTION('',(2.44929359829471E-16,0.,1.));
#22072=DIRECTION('center_axis',(-2.44929359829471E-16,-1.22460635382238E-16,
-1.));
#22073=DIRECTION('ref_axis',(2.99942050284817E-32,-1.,1.22460635382238E-16));
#22074=DIRECTION('center_axis',(-2.44929359829471E-16,-1.22460635382238E-16,
-1.));
#22075=DIRECTION('ref_axis',(2.99942050284817E-32,-1.,1.22460635382238E-16));
#22076=DIRECTION('center_axis',(-2.44929359829471E-16,-1.22460635382238E-16,
-1.));
#22077=DIRECTION('ref_axis',(2.99942050284817E-32,-1.,1.22460635382238E-16));
#22078=DIRECTION('',(4.01685164633802E-17,-0.819152044288988,0.573576436351052));
#22079=DIRECTION('center_axis',(-2.44929359829471E-16,-1.22460635382238E-16,
-1.));
#22080=DIRECTION('ref_axis',(2.99942050284817E-32,-1.,1.22460635382238E-16));
#22081=DIRECTION('center_axis',(-2.44929359829471E-16,-1.22460635382238E-16,
-1.));
#22082=DIRECTION('ref_axis',(2.99942050284817E-32,-1.,1.22460635382238E-16));
#22083=DIRECTION('center_axis',(2.44929359829471E-16,1.22460635382238E-16,
1.));
#22084=DIRECTION('ref_axis',(-2.99942050284817E-32,1.,-1.22460635382238E-16));
#22085=DIRECTION('',(-2.40802902274083E-16,0.819152044288993,-0.573576436351044));
#22086=DIRECTION('center_axis',(-2.44929359829471E-16,0.,-1.));
#22087=DIRECTION('ref_axis',(-1.,0.,2.44929359829471E-16));
#22088=DIRECTION('center_axis',(-2.44929359829471E-16,-1.22460635382238E-16,
-1.));
#22089=DIRECTION('ref_axis',(2.99942050284817E-32,-1.,1.22460635382238E-16));
#22090=DIRECTION('center_axis',(-2.44929359829471E-16,-1.22460635382238E-16,
-1.));
#22091=DIRECTION('ref_axis',(2.99942050284817E-32,-1.,1.22460635382238E-16));
#22092=DIRECTION('',(2.44929359829471E-16,0.,1.));
#22093=DIRECTION('center_axis',(-2.44929359829471E-16,-1.22460635382238E-16,
-1.));
#22094=DIRECTION('ref_axis',(2.99942050284817E-32,-1.,1.22460635382238E-16));
#22095=DIRECTION('center_axis',(-2.44929359829471E-16,-1.22460635382238E-16,
-1.));
#22096=DIRECTION('ref_axis',(2.99942050284817E-32,-1.,1.22460635382238E-16));
#22097=DIRECTION('center_axis',(-2.44929359829471E-16,-1.22460635382238E-16,
-1.));
#22098=DIRECTION('ref_axis',(2.99942050284817E-32,-1.,1.22460635382238E-16));
#22099=DIRECTION('',(4.01685164633802E-17,-0.819152044288988,0.573576436351052));
#22100=DIRECTION('center_axis',(-2.44929359829471E-16,-1.22460635382238E-16,
-1.));
#22101=DIRECTION('ref_axis',(2.99942050284817E-32,-1.,1.22460635382238E-16));
#22102=DIRECTION('center_axis',(-2.44929359829471E-16,-1.22460635382238E-16,
-1.));
#22103=DIRECTION('ref_axis',(2.99942050284817E-32,-1.,1.22460635382238E-16));
#22104=DIRECTION('center_axis',(2.44929359829471E-16,1.22460635382238E-16,
1.));
#22105=DIRECTION('ref_axis',(-2.99942050284817E-32,1.,-1.22460635382238E-16));
#22106=DIRECTION('',(-2.40802902274083E-16,0.819152044288993,-0.573576436351044));
#22107=DIRECTION('center_axis',(-2.44929359829471E-16,0.,-1.));
#22108=DIRECTION('ref_axis',(-1.,0.,2.44929359829471E-16));
#22109=DIRECTION('center_axis',(-2.44929359829471E-16,-1.22460635382238E-16,
-1.));
#22110=DIRECTION('ref_axis',(2.99942050284817E-32,-1.,1.22460635382238E-16));
#22111=DIRECTION('center_axis',(-2.44929359829471E-16,-1.22460635382238E-16,
-1.));
#22112=DIRECTION('ref_axis',(2.99942050284817E-32,-1.,1.22460635382238E-16));
#22113=DIRECTION('',(2.44929359829471E-16,0.,1.));
#22114=DIRECTION('center_axis',(-2.44929359829471E-16,-1.22460635382238E-16,
-1.));
#22115=DIRECTION('ref_axis',(2.99942050284817E-32,-1.,1.22460635382238E-16));
#22116=DIRECTION('center_axis',(-2.44929359829471E-16,-1.22460635382238E-16,
-1.));
#22117=DIRECTION('ref_axis',(2.99942050284817E-32,-1.,1.22460635382238E-16));
#22118=DIRECTION('center_axis',(-2.44929359829471E-16,-1.22460635382238E-16,
-1.));
#22119=DIRECTION('ref_axis',(2.99942050284817E-32,-1.,1.22460635382238E-16));
#22120=DIRECTION('',(4.01685164633802E-17,-0.819152044288988,0.573576436351052));
#22121=DIRECTION('center_axis',(-2.44929359829471E-16,-1.22460635382238E-16,
-1.));
#22122=DIRECTION('ref_axis',(2.99942050284817E-32,-1.,1.22460635382238E-16));
#22123=DIRECTION('center_axis',(-2.44929359829471E-16,-1.22460635382238E-16,
-1.));
#22124=DIRECTION('ref_axis',(2.99942050284817E-32,-1.,1.22460635382238E-16));
#22125=DIRECTION('center_axis',(2.44929359829471E-16,1.22460635382238E-16,
1.));
#22126=DIRECTION('ref_axis',(-2.99942050284817E-32,1.,-1.22460635382238E-16));
#22127=DIRECTION('',(-2.40802902274083E-16,0.819152044288993,-0.573576436351044));
#22128=DIRECTION('center_axis',(-2.44929359829471E-16,0.,-1.));
#22129=DIRECTION('ref_axis',(-1.,0.,2.44929359829471E-16));
#22130=DIRECTION('center_axis',(-2.44929359829471E-16,-1.22460635382238E-16,
-1.));
#22131=DIRECTION('ref_axis',(2.99942050284817E-32,-1.,1.22460635382238E-16));
#22132=DIRECTION('center_axis',(-2.44929359829471E-16,-1.22460635382238E-16,
-1.));
#22133=DIRECTION('ref_axis',(2.99942050284817E-32,-1.,1.22460635382238E-16));
#22134=DIRECTION('',(2.44929359829471E-16,0.,1.));
#22135=DIRECTION('center_axis',(-2.44929359829471E-16,-1.22460635382238E-16,
-1.));
#22136=DIRECTION('ref_axis',(2.99942050284817E-32,-1.,1.22460635382238E-16));
#22137=DIRECTION('center_axis',(-2.44929359829471E-16,-1.22460635382238E-16,
-1.));
#22138=DIRECTION('ref_axis',(2.99942050284817E-32,-1.,1.22460635382238E-16));
#22139=DIRECTION('center_axis',(-2.44929359829471E-16,-1.22460635382238E-16,
-1.));
#22140=DIRECTION('ref_axis',(2.99942050284817E-32,-1.,1.22460635382238E-16));
#22141=DIRECTION('',(4.01685164633802E-17,-0.819152044288988,0.573576436351052));
#22142=DIRECTION('center_axis',(-2.44929359829471E-16,-1.22460635382238E-16,
-1.));
#22143=DIRECTION('ref_axis',(2.99942050284817E-32,-1.,1.22460635382238E-16));
#22144=DIRECTION('center_axis',(-2.44929359829471E-16,-1.22460635382238E-16,
-1.));
#22145=DIRECTION('ref_axis',(2.99942050284817E-32,-1.,1.22460635382238E-16));
#22146=DIRECTION('center_axis',(2.44929359829471E-16,1.22460635382238E-16,
1.));
#22147=DIRECTION('ref_axis',(-2.99942050284817E-32,1.,-1.22460635382238E-16));
#22148=DIRECTION('',(-2.40802902274083E-16,0.819152044288993,-0.573576436351044));
#22149=DIRECTION('center_axis',(-2.44929359829471E-16,0.,-1.));
#22150=DIRECTION('ref_axis',(-1.,0.,2.44929359829471E-16));
#22151=DIRECTION('center_axis',(-2.44929359829471E-16,-1.22460635382238E-16,
-1.));
#22152=DIRECTION('ref_axis',(2.99942050284817E-32,-1.,1.22460635382238E-16));
#22153=DIRECTION('center_axis',(-2.44929359829471E-16,-1.22460635382238E-16,
-1.));
#22154=DIRECTION('ref_axis',(2.99942050284817E-32,-1.,1.22460635382238E-16));
#22155=DIRECTION('',(2.44929359829471E-16,0.,1.));
#22156=DIRECTION('center_axis',(-2.44929359829471E-16,-1.22460635382238E-16,
-1.));
#22157=DIRECTION('ref_axis',(2.99942050284817E-32,-1.,1.22460635382238E-16));
#22158=DIRECTION('center_axis',(-2.44929359829471E-16,-1.22460635382238E-16,
-1.));
#22159=DIRECTION('ref_axis',(2.99942050284817E-32,-1.,1.22460635382238E-16));
#22160=DIRECTION('center_axis',(-2.44929359829471E-16,-1.22460635382238E-16,
-1.));
#22161=DIRECTION('ref_axis',(2.99942050284817E-32,-1.,1.22460635382238E-16));
#22162=DIRECTION('',(4.01685164633802E-17,-0.819152044288988,0.573576436351052));
#22163=DIRECTION('center_axis',(-2.44929359829471E-16,-1.22460635382238E-16,
-1.));
#22164=DIRECTION('ref_axis',(2.99942050284817E-32,-1.,1.22460635382238E-16));
#22165=DIRECTION('center_axis',(-2.44929359829471E-16,-1.22460635382238E-16,
-1.));
#22166=DIRECTION('ref_axis',(2.99942050284817E-32,-1.,1.22460635382238E-16));
#22167=DIRECTION('center_axis',(2.44929359829471E-16,1.22460635382238E-16,
1.));
#22168=DIRECTION('ref_axis',(-2.99942050284817E-32,1.,-1.22460635382238E-16));
#22169=DIRECTION('',(-2.40802902274083E-16,0.819152044288993,-0.573576436351044));
#22170=DIRECTION('center_axis',(-2.44929359829471E-16,0.,-1.));
#22171=DIRECTION('ref_axis',(-1.,0.,2.44929359829471E-16));
#22172=DIRECTION('center_axis',(-2.44929359829471E-16,-1.22460635382238E-16,
-1.));
#22173=DIRECTION('ref_axis',(2.99942050284817E-32,-1.,1.22460635382238E-16));
#22174=DIRECTION('center_axis',(-2.44929359829471E-16,-1.22460635382238E-16,
-1.));
#22175=DIRECTION('ref_axis',(2.99942050284817E-32,-1.,1.22460635382238E-16));
#22176=DIRECTION('',(2.44929359829471E-16,0.,1.));
#22177=DIRECTION('center_axis',(-2.44929359829471E-16,-1.22460635382238E-16,
-1.));
#22178=DIRECTION('ref_axis',(2.99942050284817E-32,-1.,1.22460635382238E-16));
#22179=DIRECTION('center_axis',(-2.44929359829471E-16,-1.22460635382238E-16,
-1.));
#22180=DIRECTION('ref_axis',(2.99942050284817E-32,-1.,1.22460635382238E-16));
#22181=DIRECTION('center_axis',(-2.44929359829471E-16,-1.22460635382238E-16,
-1.));
#22182=DIRECTION('ref_axis',(2.99942050284817E-32,-1.,1.22460635382238E-16));
#22183=DIRECTION('',(4.01685164633802E-17,-0.819152044288988,0.573576436351052));
#22184=DIRECTION('center_axis',(-2.44929359829471E-16,-1.22460635382238E-16,
-1.));
#22185=DIRECTION('ref_axis',(2.99942050284817E-32,-1.,1.22460635382238E-16));
#22186=DIRECTION('center_axis',(-2.44929359829471E-16,-1.22460635382238E-16,
-1.));
#22187=DIRECTION('ref_axis',(2.99942050284817E-32,-1.,1.22460635382238E-16));
#22188=DIRECTION('center_axis',(2.44929359829471E-16,1.22460635382238E-16,
1.));
#22189=DIRECTION('ref_axis',(-2.99942050284817E-32,1.,-1.22460635382238E-16));
#22190=DIRECTION('',(-2.40802902274083E-16,0.819152044288993,-0.573576436351044));
#22191=DIRECTION('center_axis',(2.44929359829471E-16,0.,1.));
#22192=DIRECTION('ref_axis',(1.,0.,-2.44929359829471E-16));
#22193=DIRECTION('center_axis',(-2.44929359829471E-16,0.,-1.));
#22194=DIRECTION('ref_axis',(-1.,0.,2.44929359829471E-16));
#22195=DIRECTION('center_axis',(-2.44929359829471E-16,0.,-1.));
#22196=DIRECTION('ref_axis',(-1.,0.,2.44929359829471E-16));
#22197=DIRECTION('center_axis',(-2.44929359829471E-16,0.,-1.));
#22198=DIRECTION('ref_axis',(-1.,0.,2.44929359829471E-16));
#22199=DIRECTION('center_axis',(-2.44929359829471E-16,0.,-1.));
#22200=DIRECTION('ref_axis',(-1.,0.,2.44929359829471E-16));
#22201=DIRECTION('center_axis',(-2.44929359829471E-16,0.,-1.));
#22202=DIRECTION('ref_axis',(-1.,0.,2.44929359829471E-16));
#22203=DIRECTION('center_axis',(-2.44929359829471E-16,0.,-1.));
#22204=DIRECTION('ref_axis',(-1.,0.,2.44929359829471E-16));
#22205=DIRECTION('center_axis',(-2.44929359829471E-16,0.,-1.));
#22206=DIRECTION('ref_axis',(-1.,0.,2.44929359829471E-16));
#22207=DIRECTION('center_axis',(-2.44929359829471E-16,0.,-1.));
#22208=DIRECTION('ref_axis',(-1.,0.,2.44929359829471E-16));
#22209=DIRECTION('center_axis',(-2.44929359829471E-16,0.,-1.));
#22210=DIRECTION('ref_axis',(-1.,0.,2.44929359829471E-16));
#22211=DIRECTION('center_axis',(-2.44929359829471E-16,0.,-1.));
#22212=DIRECTION('ref_axis',(-1.,0.,2.44929359829471E-16));
#22213=DIRECTION('center_axis',(-2.44929359829471E-16,0.,-1.));
#22214=DIRECTION('ref_axis',(-1.,0.,2.44929359829471E-16));
#22215=DIRECTION('center_axis',(-2.44929359829471E-16,0.,-1.));
#22216=DIRECTION('ref_axis',(-1.,0.,2.44929359829471E-16));
#22217=DIRECTION('center_axis',(-2.44929359829471E-16,0.,-1.));
#22218=DIRECTION('ref_axis',(-1.,0.,2.44929359829471E-16));
#22219=DIRECTION('center_axis',(-2.44929359829471E-16,0.,-1.));
#22220=DIRECTION('ref_axis',(-1.,0.,2.44929359829471E-16));
#22221=DIRECTION('center_axis',(-2.44929359829471E-16,0.,-1.));
#22222=DIRECTION('ref_axis',(-1.,0.,2.44929359829471E-16));
#22223=DIRECTION('center_axis',(-2.44929359829471E-16,0.,-1.));
#22224=DIRECTION('ref_axis',(-1.,0.,2.44929359829471E-16));
#22225=DIRECTION('center_axis',(-2.44929359829471E-16,0.,-1.));
#22226=DIRECTION('ref_axis',(-1.,0.,2.44929359829471E-16));
#22227=DIRECTION('center_axis',(-2.44929359829471E-16,0.,-1.));
#22228=DIRECTION('ref_axis',(-1.,0.,2.44929359829471E-16));
#22229=DIRECTION('center_axis',(-2.44929359829471E-16,0.,-1.));
#22230=DIRECTION('ref_axis',(-1.,0.,2.44929359829471E-16));
#22231=DIRECTION('center_axis',(-2.44929359829471E-16,0.,-1.));
#22232=DIRECTION('ref_axis',(-1.,0.,2.44929359829471E-16));
#22233=DIRECTION('center_axis',(-2.44929359829471E-16,0.,-1.));
#22234=DIRECTION('ref_axis',(-1.,0.,2.44929359829471E-16));
#22235=DIRECTION('center_axis',(-2.44929359829471E-16,0.,-1.));
#22236=DIRECTION('ref_axis',(-1.,0.,2.44929359829471E-16));
#22237=DIRECTION('center_axis',(-2.44929359829471E-16,0.,-1.));
#22238=DIRECTION('ref_axis',(-1.,0.,2.44929359829471E-16));
#22239=DIRECTION('center_axis',(-2.44929359829471E-16,0.,-1.));
#22240=DIRECTION('ref_axis',(-1.,0.,2.44929359829471E-16));
#22241=DIRECTION('center_axis',(-2.44929359829471E-16,0.,-1.));
#22242=DIRECTION('ref_axis',(-1.,0.,2.44929359829471E-16));
#22243=DIRECTION('center_axis',(-2.44929359829471E-16,0.,-1.));
#22244=DIRECTION('ref_axis',(-1.,0.,2.44929359829471E-16));
#22245=DIRECTION('center_axis',(-2.44929359829471E-16,0.,-1.));
#22246=DIRECTION('ref_axis',(-1.,0.,2.44929359829471E-16));
#22247=DIRECTION('center_axis',(-2.44929359829471E-16,0.,-1.));
#22248=DIRECTION('ref_axis',(-1.,0.,2.44929359829471E-16));
#22249=DIRECTION('center_axis',(-2.44929359829471E-16,0.,-1.));
#22250=DIRECTION('ref_axis',(-1.,0.,2.44929359829471E-16));
#22251=DIRECTION('center_axis',(-2.44929359829471E-16,0.,-1.));
#22252=DIRECTION('ref_axis',(-1.,0.,2.44929359829471E-16));
#22253=DIRECTION('center_axis',(-2.44929359829471E-16,0.,-1.));
#22254=DIRECTION('ref_axis',(-1.,0.,2.44929359829471E-16));
#22255=DIRECTION('center_axis',(-2.44929359829471E-16,0.,-1.));
#22256=DIRECTION('ref_axis',(-1.,0.,2.44929359829471E-16));
#22257=DIRECTION('center_axis',(-2.44929359829471E-16,0.,-1.));
#22258=DIRECTION('ref_axis',(-1.,0.,2.44929359829471E-16));
#22259=DIRECTION('center_axis',(-2.44929359829471E-16,0.,-1.));
#22260=DIRECTION('ref_axis',(-1.,0.,2.44929359829471E-16));
#22261=DIRECTION('center_axis',(-2.44929359829471E-16,0.,-1.));
#22262=DIRECTION('ref_axis',(-1.,0.,2.44929359829471E-16));
#22263=DIRECTION('center_axis',(-2.44929359829471E-16,0.,-1.));
#22264=DIRECTION('ref_axis',(-1.,0.,2.44929359829471E-16));
#22265=DIRECTION('center_axis',(-2.44929359829471E-16,0.,-1.));
#22266=DIRECTION('ref_axis',(-1.,0.,2.44929359829471E-16));
#22267=DIRECTION('center_axis',(-2.44929359829471E-16,0.,-1.));
#22268=DIRECTION('ref_axis',(-1.,0.,2.44929359829471E-16));
#22269=DIRECTION('center_axis',(-2.44929359829471E-16,0.,-1.));
#22270=DIRECTION('ref_axis',(-1.,0.,2.44929359829471E-16));
#22271=DIRECTION('',(0.70710678118655,8.65956056235496E-17,-0.707106781186545));
#22272=DIRECTION('center_axis',(-2.44929359829471E-16,0.,-1.));
#22273=DIRECTION('ref_axis',(-1.,0.,2.44929359829471E-16));
#22274=DIRECTION('center_axis',(-2.44929359829471E-16,0.,-1.));
#22275=DIRECTION('ref_axis',(-1.,0.,2.44929359829471E-16));
#22276=DIRECTION('center_axis',(-2.44929359829471E-16,0.,-1.));
#22277=DIRECTION('ref_axis',(-1.,0.,2.44929359829471E-16));
#22278=DIRECTION('center_axis',(-2.44929359829471E-16,0.,-1.));
#22279=DIRECTION('ref_axis',(-1.,0.,2.44929359829471E-16));
#22280=DIRECTION('center_axis',(-2.44929359829471E-16,0.,-1.));
#22281=DIRECTION('ref_axis',(-1.,0.,2.44929359829471E-16));
#22282=DIRECTION('center_axis',(-2.44929359829471E-16,0.,-1.));
#22283=DIRECTION('ref_axis',(-1.,0.,2.44929359829471E-16));
#22284=DIRECTION('center_axis',(-2.44929359829471E-16,0.,-1.));
#22285=DIRECTION('ref_axis',(-1.,0.,2.44929359829471E-16));
#22286=DIRECTION('center_axis',(-2.44929359829471E-16,0.,-1.));
#22287=DIRECTION('ref_axis',(-1.,0.,2.44929359829471E-16));
#22288=DIRECTION('center_axis',(-2.44929359829471E-16,0.,-1.));
#22289=DIRECTION('ref_axis',(-1.,0.,2.44929359829471E-16));
#22290=DIRECTION('center_axis',(-2.44929359829471E-16,0.,-1.));
#22291=DIRECTION('ref_axis',(-1.,0.,2.44929359829471E-16));
#22292=DIRECTION('center_axis',(-2.44929359829471E-16,0.,-1.));
#22293=DIRECTION('ref_axis',(-1.,0.,2.44929359829471E-16));
#22294=DIRECTION('center_axis',(-2.44929359829471E-16,0.,-1.));
#22295=DIRECTION('ref_axis',(-1.,0.,2.44929359829471E-16));
#22296=DIRECTION('center_axis',(-2.44929359829471E-16,0.,-1.));
#22297=DIRECTION('ref_axis',(-1.,0.,2.44929359829471E-16));
#22298=DIRECTION('center_axis',(-2.44929359829471E-16,0.,-1.));
#22299=DIRECTION('ref_axis',(-1.,0.,2.44929359829471E-16));
#22300=DIRECTION('center_axis',(-2.44929359829471E-16,0.,-1.));
#22301=DIRECTION('ref_axis',(-1.,0.,2.44929359829471E-16));
#22302=DIRECTION('center_axis',(-2.44929359829471E-16,0.,-1.));
#22303=DIRECTION('ref_axis',(-1.,0.,2.44929359829471E-16));
#22304=DIRECTION('center_axis',(-2.44929359829471E-16,0.,-1.));
#22305=DIRECTION('ref_axis',(-1.,0.,2.44929359829471E-16));
#22306=DIRECTION('center_axis',(-2.44929359829471E-16,0.,-1.));
#22307=DIRECTION('ref_axis',(-1.,0.,2.44929359829471E-16));
#22308=DIRECTION('center_axis',(-2.44929359829471E-16,0.,-1.));
#22309=DIRECTION('ref_axis',(-1.,0.,2.44929359829471E-16));
#22310=DIRECTION('center_axis',(-2.44929359829471E-16,0.,-1.));
#22311=DIRECTION('ref_axis',(-1.,0.,2.44929359829471E-16));
#22312=DIRECTION('center_axis',(-2.44929359829471E-16,0.,-1.));
#22313=DIRECTION('ref_axis',(-1.,0.,2.44929359829471E-16));
#22314=DIRECTION('center_axis',(-2.44929359829471E-16,0.,-1.));
#22315=DIRECTION('ref_axis',(-1.,0.,2.44929359829471E-16));
#22316=DIRECTION('center_axis',(-2.44929359829471E-16,0.,-1.));
#22317=DIRECTION('ref_axis',(-1.,0.,2.44929359829471E-16));
#22318=DIRECTION('center_axis',(-2.44929359829471E-16,0.,-1.));
#22319=DIRECTION('ref_axis',(-1.,0.,2.44929359829471E-16));
#22320=DIRECTION('center_axis',(-2.44929359829471E-16,0.,-1.));
#22321=DIRECTION('ref_axis',(-1.,0.,2.44929359829471E-16));
#22322=DIRECTION('center_axis',(-2.44929359829471E-16,0.,-1.));
#22323=DIRECTION('ref_axis',(-1.,0.,2.44929359829471E-16));
#22324=DIRECTION('center_axis',(-2.44929359829471E-16,0.,-1.));
#22325=DIRECTION('ref_axis',(-1.,0.,2.44929359829471E-16));
#22326=DIRECTION('center_axis',(-2.44929359829471E-16,0.,-1.));
#22327=DIRECTION('ref_axis',(-1.,0.,2.44929359829471E-16));
#22328=DIRECTION('center_axis',(-2.44929359829471E-16,0.,-1.));
#22329=DIRECTION('ref_axis',(-1.,0.,2.44929359829471E-16));
#22330=DIRECTION('center_axis',(-2.44929359829471E-16,0.,-1.));
#22331=DIRECTION('ref_axis',(-1.,0.,2.44929359829471E-16));
#22332=DIRECTION('center_axis',(-2.44929359829471E-16,0.,-1.));
#22333=DIRECTION('ref_axis',(-1.,0.,2.44929359829471E-16));
#22334=DIRECTION('center_axis',(-2.44929359829471E-16,0.,-1.));
#22335=DIRECTION('ref_axis',(-1.,0.,2.44929359829471E-16));
#22336=DIRECTION('center_axis',(-2.44929359829471E-16,0.,-1.));
#22337=DIRECTION('ref_axis',(-1.,0.,2.44929359829471E-16));
#22338=DIRECTION('center_axis',(-2.44929359829471E-16,0.,-1.));
#22339=DIRECTION('ref_axis',(-1.,0.,2.44929359829471E-16));
#22340=DIRECTION('center_axis',(-2.44929359829471E-16,0.,-1.));
#22341=DIRECTION('ref_axis',(-1.,0.,2.44929359829471E-16));
#22342=DIRECTION('center_axis',(-2.44929359829471E-16,0.,-1.));
#22343=DIRECTION('ref_axis',(-1.,0.,2.44929359829471E-16));
#22344=DIRECTION('center_axis',(-2.44929359829471E-16,0.,-1.));
#22345=DIRECTION('ref_axis',(-1.,0.,2.44929359829471E-16));
#22346=DIRECTION('center_axis',(-2.44929359829471E-16,0.,-1.));
#22347=DIRECTION('ref_axis',(-1.,0.,2.44929359829471E-16));
#22348=DIRECTION('center_axis',(-2.44929359829471E-16,0.,-1.));
#22349=DIRECTION('ref_axis',(-1.,0.,2.44929359829471E-16));
#22350=DIRECTION('center_axis',(-2.44929359829471E-16,0.,-1.));
#22351=DIRECTION('ref_axis',(-1.,0.,2.44929359829471E-16));
#22352=DIRECTION('center_axis',(-2.44929359829471E-16,0.,-1.));
#22353=DIRECTION('ref_axis',(-1.,0.,2.44929359829471E-16));
#22354=DIRECTION('center_axis',(-2.44929359829471E-16,0.,-1.));
#22355=DIRECTION('ref_axis',(-1.,0.,2.44929359829471E-16));
#22356=DIRECTION('center_axis',(-2.44929359829471E-16,0.,-1.));
#22357=DIRECTION('ref_axis',(-1.,0.,2.44929359829471E-16));
#22358=DIRECTION('center_axis',(-2.44929359829471E-16,0.,-1.));
#22359=DIRECTION('ref_axis',(-1.,0.,2.44929359829471E-16));
#22360=DIRECTION('center_axis',(-2.44929359829471E-16,0.,-1.));
#22361=DIRECTION('ref_axis',(-1.,0.,2.44929359829471E-16));
#22362=DIRECTION('center_axis',(-2.44929359829471E-16,0.,-1.));
#22363=DIRECTION('ref_axis',(-1.,0.,2.44929359829471E-16));
#22364=DIRECTION('center_axis',(-2.44929359829471E-16,0.,-1.));
#22365=DIRECTION('ref_axis',(-1.,0.,2.44929359829471E-16));
#22366=DIRECTION('center_axis',(-2.44929359829471E-16,0.,-1.));
#22367=DIRECTION('ref_axis',(-1.,0.,2.44929359829471E-16));
#22368=DIRECTION('center_axis',(-2.44929359829471E-16,0.,-1.));
#22369=DIRECTION('ref_axis',(-1.,0.,2.44929359829471E-16));
#22370=DIRECTION('center_axis',(-2.44929359829471E-16,0.,-1.));
#22371=DIRECTION('ref_axis',(-1.,0.,2.44929359829471E-16));
#22372=DIRECTION('center_axis',(-2.44929359829471E-16,0.,-1.));
#22373=DIRECTION('ref_axis',(-1.,0.,2.44929359829471E-16));
#22374=DIRECTION('center_axis',(-2.44929359829471E-16,0.,-1.));
#22375=DIRECTION('ref_axis',(-1.,0.,2.44929359829471E-16));
#22376=DIRECTION('center_axis',(-2.44929359829471E-16,0.,-1.));
#22377=DIRECTION('ref_axis',(-1.,0.,2.44929359829471E-16));
#22378=DIRECTION('center_axis',(-2.44929359829471E-16,0.,-1.));
#22379=DIRECTION('ref_axis',(-1.,0.,2.44929359829471E-16));
#22380=DIRECTION('center_axis',(-2.44929359829471E-16,0.,-1.));
#22381=DIRECTION('ref_axis',(-1.,0.,2.44929359829471E-16));
#22382=DIRECTION('center_axis',(-2.44929359829471E-16,0.,-1.));
#22383=DIRECTION('ref_axis',(-1.,0.,2.44929359829471E-16));
#22384=DIRECTION('center_axis',(-2.44929359829471E-16,0.,-1.));
#22385=DIRECTION('ref_axis',(-1.,0.,2.44929359829471E-16));
#22386=DIRECTION('center_axis',(-2.44929359829471E-16,0.,-1.));
#22387=DIRECTION('ref_axis',(-1.,0.,2.44929359829471E-16));
#22388=DIRECTION('center_axis',(-2.44929359829471E-16,0.,-1.));
#22389=DIRECTION('ref_axis',(-1.,0.,2.44929359829471E-16));
#22390=DIRECTION('center_axis',(-2.44929359829471E-16,0.,-1.));
#22391=DIRECTION('ref_axis',(-1.,0.,2.44929359829471E-16));
#22392=DIRECTION('center_axis',(-2.44929359829471E-16,0.,-1.));
#22393=DIRECTION('ref_axis',(-1.,0.,2.44929359829471E-16));
#22394=DIRECTION('center_axis',(-2.44929359829471E-16,0.,-1.));
#22395=DIRECTION('ref_axis',(-1.,0.,2.44929359829471E-16));
#22396=DIRECTION('center_axis',(-2.44929359829471E-16,0.,-1.));
#22397=DIRECTION('ref_axis',(-1.,0.,2.44929359829471E-16));
#22398=DIRECTION('center_axis',(-2.44929359829471E-16,0.,-1.));
#22399=DIRECTION('ref_axis',(-1.,0.,2.44929359829471E-16));
#22400=DIRECTION('center_axis',(-2.44929359829471E-16,0.,-1.));
#22401=DIRECTION('ref_axis',(-1.,0.,2.44929359829471E-16));
#22402=DIRECTION('center_axis',(-2.44929359829471E-16,0.,-1.));
#22403=DIRECTION('ref_axis',(-1.,0.,2.44929359829471E-16));
#22404=DIRECTION('center_axis',(-2.44929359829471E-16,0.,-1.));
#22405=DIRECTION('ref_axis',(-1.,0.,2.44929359829471E-16));
#22406=DIRECTION('center_axis',(-2.44929359829471E-16,0.,-1.));
#22407=DIRECTION('ref_axis',(-1.,0.,2.44929359829471E-16));
#22408=DIRECTION('center_axis',(-2.44929359829471E-16,0.,-1.));
#22409=DIRECTION('ref_axis',(-1.,0.,2.44929359829471E-16));
#22410=DIRECTION('center_axis',(-2.44929359829471E-16,0.,-1.));
#22411=DIRECTION('ref_axis',(-1.,0.,2.44929359829471E-16));
#22412=DIRECTION('center_axis',(-2.44929359829471E-16,0.,-1.));
#22413=DIRECTION('ref_axis',(-1.,0.,2.44929359829471E-16));
#22414=DIRECTION('center_axis',(-2.44929359829471E-16,0.,-1.));
#22415=DIRECTION('ref_axis',(-1.,0.,2.44929359829471E-16));
#22416=DIRECTION('center_axis',(-2.44929359829471E-16,0.,-1.));
#22417=DIRECTION('ref_axis',(-1.,0.,2.44929359829471E-16));
#22418=DIRECTION('center_axis',(-2.44929359829471E-16,0.,-1.));
#22419=DIRECTION('ref_axis',(-1.,0.,2.44929359829471E-16));
#22420=DIRECTION('center_axis',(-2.44929359829471E-16,0.,-1.));
#22421=DIRECTION('ref_axis',(-1.,0.,2.44929359829471E-16));
#22422=DIRECTION('center_axis',(-2.44929359829471E-16,0.,-1.));
#22423=DIRECTION('ref_axis',(-1.,0.,2.44929359829471E-16));
#22424=DIRECTION('center_axis',(-2.44929359829471E-16,0.,-1.));
#22425=DIRECTION('ref_axis',(-1.,0.,2.44929359829471E-16));
#22426=DIRECTION('center_axis',(-2.44929359829471E-16,0.,-1.));
#22427=DIRECTION('ref_axis',(-1.,0.,2.44929359829471E-16));
#22428=DIRECTION('center_axis',(-2.44929359829471E-16,0.,-1.));
#22429=DIRECTION('ref_axis',(-1.,0.,2.44929359829471E-16));
#22430=DIRECTION('',(-0.70710678118655,8.65956056235496E-17,0.707106781186545));
#22431=DIRECTION('center_axis',(-2.44929359829471E-16,0.,-1.));
#22432=DIRECTION('ref_axis',(-1.,0.,2.44929359829471E-16));
#22433=DIRECTION('center_axis',(-2.44929359829471E-16,0.,-1.));
#22434=DIRECTION('ref_axis',(-1.,0.,2.44929359829471E-16));
#22435=DIRECTION('center_axis',(-2.44929359829471E-16,0.,-1.));
#22436=DIRECTION('ref_axis',(-1.,0.,2.44929359829471E-16));
#22437=DIRECTION('center_axis',(-2.44929359829471E-16,0.,-1.));
#22438=DIRECTION('ref_axis',(-1.,0.,2.44929359829471E-16));
#22439=DIRECTION('center_axis',(-2.44929359829471E-16,0.,-1.));
#22440=DIRECTION('ref_axis',(-1.,0.,2.44929359829471E-16));
#22441=DIRECTION('center_axis',(-2.44929359829471E-16,0.,-1.));
#22442=DIRECTION('ref_axis',(-1.,0.,2.44929359829471E-16));
#22443=DIRECTION('center_axis',(-2.44929359829471E-16,0.,-1.));
#22444=DIRECTION('ref_axis',(-1.,0.,2.44929359829471E-16));
#22445=DIRECTION('center_axis',(-2.44929359829471E-16,0.,-1.));
#22446=DIRECTION('ref_axis',(-1.,0.,2.44929359829471E-16));
#22447=DIRECTION('center_axis',(-2.44929359829471E-16,0.,-1.));
#22448=DIRECTION('ref_axis',(-1.,0.,2.44929359829471E-16));
#22449=DIRECTION('center_axis',(-2.44929359829471E-16,0.,-1.));
#22450=DIRECTION('ref_axis',(-1.,0.,2.44929359829471E-16));
#22451=DIRECTION('center_axis',(-2.44929359829471E-16,0.,-1.));
#22452=DIRECTION('ref_axis',(-1.,0.,2.44929359829471E-16));
#22453=DIRECTION('center_axis',(-2.44929359829471E-16,0.,-1.));
#22454=DIRECTION('ref_axis',(-1.,0.,2.44929359829471E-16));
#22455=DIRECTION('center_axis',(-2.44929359829471E-16,0.,-1.));
#22456=DIRECTION('ref_axis',(-1.,0.,2.44929359829471E-16));
#22457=DIRECTION('center_axis',(-2.44929359829471E-16,0.,-1.));
#22458=DIRECTION('ref_axis',(-1.,0.,2.44929359829471E-16));
#22459=DIRECTION('center_axis',(-2.44929359829471E-16,0.,-1.));
#22460=DIRECTION('ref_axis',(-1.,0.,2.44929359829471E-16));
#22461=DIRECTION('center_axis',(-2.44929359829471E-16,0.,-1.));
#22462=DIRECTION('ref_axis',(-1.,0.,2.44929359829471E-16));
#22463=DIRECTION('center_axis',(-2.44929359829471E-16,0.,-1.));
#22464=DIRECTION('ref_axis',(-1.,0.,2.44929359829471E-16));
#22465=DIRECTION('center_axis',(-2.44929359829471E-16,0.,-1.));
#22466=DIRECTION('ref_axis',(-1.,0.,2.44929359829471E-16));
#22467=DIRECTION('center_axis',(-2.44929359829471E-16,0.,-1.));
#22468=DIRECTION('ref_axis',(-1.,0.,2.44929359829471E-16));
#22469=DIRECTION('center_axis',(-2.44929359829471E-16,0.,-1.));
#22470=DIRECTION('ref_axis',(-1.,0.,2.44929359829471E-16));
#22471=DIRECTION('center_axis',(-2.44929359829471E-16,0.,-1.));
#22472=DIRECTION('ref_axis',(-1.,0.,2.44929359829471E-16));
#22473=DIRECTION('center_axis',(-2.44929359829471E-16,0.,-1.));
#22474=DIRECTION('ref_axis',(-1.,0.,2.44929359829471E-16));
#22475=DIRECTION('center_axis',(-2.44929359829471E-16,0.,-1.));
#22476=DIRECTION('ref_axis',(-1.,0.,2.44929359829471E-16));
#22477=DIRECTION('center_axis',(-2.44929359829471E-16,0.,-1.));
#22478=DIRECTION('ref_axis',(-1.,0.,2.44929359829471E-16));
#22479=DIRECTION('center_axis',(-2.44929359829471E-16,0.,-1.));
#22480=DIRECTION('ref_axis',(-1.,0.,2.44929359829471E-16));
#22481=DIRECTION('center_axis',(-2.44929359829471E-16,0.,-1.));
#22482=DIRECTION('ref_axis',(-1.,0.,2.44929359829471E-16));
#22483=DIRECTION('center_axis',(-2.44929359829471E-16,0.,-1.));
#22484=DIRECTION('ref_axis',(-1.,0.,2.44929359829471E-16));
#22485=DIRECTION('center_axis',(-2.44929359829471E-16,0.,-1.));
#22486=DIRECTION('ref_axis',(-1.,0.,2.44929359829471E-16));
#22487=DIRECTION('center_axis',(-2.44929359829471E-16,0.,-1.));
#22488=DIRECTION('ref_axis',(-1.,0.,2.44929359829471E-16));
#22489=DIRECTION('center_axis',(-2.44929359829471E-16,0.,-1.));
#22490=DIRECTION('ref_axis',(-1.,0.,2.44929359829471E-16));
#22491=DIRECTION('center_axis',(-2.44929359829471E-16,0.,-1.));
#22492=DIRECTION('ref_axis',(-1.,0.,2.44929359829471E-16));
#22493=DIRECTION('center_axis',(-2.44929359829471E-16,0.,-1.));
#22494=DIRECTION('ref_axis',(-1.,0.,2.44929359829471E-16));
#22495=DIRECTION('center_axis',(-2.44929359829471E-16,0.,-1.));
#22496=DIRECTION('ref_axis',(-1.,0.,2.44929359829471E-16));
#22497=DIRECTION('center_axis',(-2.44929359829471E-16,0.,-1.));
#22498=DIRECTION('ref_axis',(-1.,0.,2.44929359829471E-16));
#22499=DIRECTION('center_axis',(-2.44929359829471E-16,0.,-1.));
#22500=DIRECTION('ref_axis',(-1.,0.,2.44929359829471E-16));
#22501=DIRECTION('center_axis',(-2.44929359829471E-16,0.,-1.));
#22502=DIRECTION('ref_axis',(-1.,0.,2.44929359829471E-16));
#22503=DIRECTION('center_axis',(-2.44929359829471E-16,0.,-1.));
#22504=DIRECTION('ref_axis',(-1.,0.,2.44929359829471E-16));
#22505=DIRECTION('center_axis',(-2.44929359829471E-16,0.,-1.));
#22506=DIRECTION('ref_axis',(-1.,0.,2.44929359829471E-16));
#22507=DIRECTION('center_axis',(-2.44929359829471E-16,0.,-1.));
#22508=DIRECTION('ref_axis',(-1.,0.,2.44929359829471E-16));
#22509=DIRECTION('center_axis',(-2.44929359829471E-16,0.,-1.));
#22510=DIRECTION('ref_axis',(-1.,0.,2.44929359829471E-16));
#22511=DIRECTION('',(2.44929359829471E-16,0.,1.));
#22512=DIRECTION('center_axis',(-2.44929359829471E-16,0.,-1.));
#22513=DIRECTION('ref_axis',(-1.,0.,2.44929359829471E-16));
#22514=DIRECTION('',(-2.44929359829471E-16,0.,-1.));
#22515=DIRECTION('',(-2.44929359829471E-16,0.,-1.));
#22516=DIRECTION('center_axis',(-2.44929359829471E-16,0.,-1.));
#22517=DIRECTION('ref_axis',(-1.,0.,2.44929359829471E-16));
#22518=DIRECTION('',(-2.44929359829471E-16,0.,-1.));
#22519=DIRECTION('',(-2.44929359829471E-16,0.,-1.));
#22520=DIRECTION('center_axis',(-2.44929359829471E-16,0.,-1.));
#22521=DIRECTION('ref_axis',(-1.,0.,2.44929359829471E-16));
#22522=DIRECTION('',(-2.44929359829471E-16,0.,-1.));
#22523=DIRECTION('',(-2.44929359829471E-16,0.,-1.));
#22524=DIRECTION('center_axis',(-2.44929359829471E-16,0.,-1.));
#22525=DIRECTION('ref_axis',(-1.,0.,2.44929359829471E-16));
#22526=DIRECTION('',(-2.44929359829471E-16,0.,-1.));
#22527=DIRECTION('',(-2.44929359829471E-16,0.,-1.));
#22528=DIRECTION('center_axis',(-2.44929359829471E-16,0.,-1.));
#22529=DIRECTION('ref_axis',(-1.,0.,2.44929359829471E-16));
#22530=DIRECTION('',(-2.44929359829471E-16,0.,-1.));
#22531=DIRECTION('',(-2.44929359829471E-16,0.,-1.));
#22532=DIRECTION('center_axis',(-2.44929359829471E-16,0.,-1.));
#22533=DIRECTION('ref_axis',(-1.,0.,2.44929359829471E-16));
#22534=DIRECTION('',(-2.44929359829471E-16,0.,-1.));
#22535=DIRECTION('',(-2.44929359829471E-16,0.,-1.));
#22536=DIRECTION('center_axis',(-2.44929359829471E-16,0.,-1.));
#22537=DIRECTION('ref_axis',(-1.,0.,2.44929359829471E-16));
#22538=DIRECTION('',(-2.44929359829471E-16,0.,-1.));
#22539=DIRECTION('',(-2.44929359829471E-16,0.,-1.));
#22540=DIRECTION('center_axis',(-2.44929359829471E-16,0.,-1.));
#22541=DIRECTION('ref_axis',(-1.,0.,2.44929359829471E-16));
#22542=DIRECTION('',(-2.44929359829471E-16,0.,-1.));
#22543=DIRECTION('',(-2.44929359829471E-16,0.,-1.));
#22544=DIRECTION('center_axis',(-2.44929359829471E-16,0.,-1.));
#22545=DIRECTION('ref_axis',(-1.,0.,2.44929359829471E-16));
#22546=DIRECTION('',(-2.44929359829471E-16,0.,-1.));
#22547=DIRECTION('',(-2.44929359829471E-16,0.,-1.));
#22548=DIRECTION('center_axis',(-2.44929359829471E-16,0.,-1.));
#22549=DIRECTION('ref_axis',(-1.,0.,2.44929359829471E-16));
#22550=DIRECTION('',(-2.44929359829471E-16,0.,-1.));
#22551=DIRECTION('',(-2.44929359829471E-16,0.,-1.));
#22552=DIRECTION('center_axis',(-2.44929359829471E-16,0.,-1.));
#22553=DIRECTION('ref_axis',(-1.,0.,2.44929359829471E-16));
#22554=DIRECTION('',(-2.44929359829471E-16,0.,-1.));
#22555=DIRECTION('',(-2.44929359829471E-16,0.,-1.));
#22556=DIRECTION('center_axis',(-2.44929359829471E-16,0.,-1.));
#22557=DIRECTION('ref_axis',(-1.,0.,2.44929359829471E-16));
#22558=DIRECTION('',(-2.44929359829471E-16,0.,-1.));
#22559=DIRECTION('',(-2.44929359829471E-16,0.,-1.));
#22560=DIRECTION('center_axis',(-2.44929359829471E-16,0.,-1.));
#22561=DIRECTION('ref_axis',(-1.,0.,2.44929359829471E-16));
#22562=DIRECTION('',(-2.44929359829471E-16,0.,-1.));
#22563=DIRECTION('',(-2.44929359829471E-16,0.,-1.));
#22564=DIRECTION('center_axis',(-2.44929359829471E-16,0.,-1.));
#22565=DIRECTION('ref_axis',(-1.,0.,2.44929359829471E-16));
#22566=DIRECTION('',(-2.44929359829471E-16,0.,-1.));
#22567=DIRECTION('',(-2.44929359829471E-16,0.,-1.));
#22568=DIRECTION('center_axis',(-2.44929359829471E-16,0.,-1.));
#22569=DIRECTION('ref_axis',(-1.,0.,2.44929359829471E-16));
#22570=DIRECTION('',(-2.44929359829471E-16,0.,-1.));
#22571=DIRECTION('',(-2.44929359829471E-16,0.,-1.));
#22572=DIRECTION('center_axis',(-2.44929359829471E-16,0.,-1.));
#22573=DIRECTION('ref_axis',(-1.,0.,2.44929359829471E-16));
#22574=DIRECTION('',(-2.44929359829471E-16,0.,-1.));
#22575=DIRECTION('',(-2.44929359829471E-16,0.,-1.));
#22576=DIRECTION('center_axis',(-2.44929359829471E-16,0.,-1.));
#22577=DIRECTION('ref_axis',(-1.,0.,2.44929359829471E-16));
#22578=DIRECTION('',(-2.44929359829471E-16,0.,-1.));
#22579=DIRECTION('',(-2.44929359829471E-16,0.,-1.));
#22580=DIRECTION('center_axis',(-2.44929359829471E-16,0.,-1.));
#22581=DIRECTION('ref_axis',(-1.,0.,2.44929359829471E-16));
#22582=DIRECTION('',(-2.44929359829471E-16,0.,-1.));
#22583=DIRECTION('',(-2.44929359829471E-16,0.,-1.));
#22584=DIRECTION('center_axis',(-2.44929359829471E-16,0.,-1.));
#22585=DIRECTION('ref_axis',(-1.,0.,2.44929359829471E-16));
#22586=DIRECTION('',(-2.44929359829471E-16,0.,-1.));
#22587=DIRECTION('',(-2.44929359829471E-16,0.,-1.));
#22588=DIRECTION('center_axis',(-2.44929359829471E-16,0.,-1.));
#22589=DIRECTION('ref_axis',(-1.,0.,2.44929359829471E-16));
#22590=DIRECTION('',(-2.44929359829471E-16,0.,-1.));
#22591=DIRECTION('',(-2.44929359829471E-16,0.,-1.));
#22592=DIRECTION('center_axis',(-2.44929359829471E-16,0.,-1.));
#22593=DIRECTION('ref_axis',(-1.,0.,2.44929359829471E-16));
#22594=DIRECTION('',(-2.44929359829471E-16,0.,-1.));
#22595=DIRECTION('',(-2.44929359829471E-16,0.,-1.));
#22596=DIRECTION('center_axis',(-2.44929359829471E-16,0.,-1.));
#22597=DIRECTION('ref_axis',(-1.,0.,2.44929359829471E-16));
#22598=DIRECTION('',(-2.44929359829471E-16,0.,-1.));
#22599=DIRECTION('',(-2.44929359829471E-16,0.,-1.));
#22600=DIRECTION('center_axis',(-2.44929359829471E-16,0.,-1.));
#22601=DIRECTION('ref_axis',(-1.,0.,2.44929359829471E-16));
#22602=DIRECTION('',(-2.44929359829471E-16,0.,-1.));
#22603=DIRECTION('',(-2.44929359829471E-16,0.,-1.));
#22604=DIRECTION('center_axis',(-2.44929359829471E-16,0.,-1.));
#22605=DIRECTION('ref_axis',(-1.,0.,2.44929359829471E-16));
#22606=DIRECTION('',(-2.44929359829471E-16,0.,-1.));
#22607=DIRECTION('',(-2.44929359829471E-16,0.,-1.));
#22608=DIRECTION('center_axis',(-2.44929359829471E-16,0.,-1.));
#22609=DIRECTION('ref_axis',(-1.,0.,2.44929359829471E-16));
#22610=DIRECTION('',(-2.44929359829471E-16,0.,-1.));
#22611=DIRECTION('',(-2.44929359829471E-16,0.,-1.));
#22612=DIRECTION('center_axis',(-2.44929359829471E-16,0.,-1.));
#22613=DIRECTION('ref_axis',(-1.,0.,2.44929359829471E-16));
#22614=DIRECTION('',(-2.44929359829471E-16,0.,-1.));
#22615=DIRECTION('',(-2.44929359829471E-16,0.,-1.));
#22616=DIRECTION('center_axis',(-2.44929359829471E-16,0.,-1.));
#22617=DIRECTION('ref_axis',(-1.,0.,2.44929359829471E-16));
#22618=DIRECTION('',(-2.44929359829471E-16,0.,-1.));
#22619=DIRECTION('',(-2.44929359829471E-16,0.,-1.));
#22620=DIRECTION('center_axis',(-2.44929359829471E-16,0.,-1.));
#22621=DIRECTION('ref_axis',(-1.,0.,2.44929359829471E-16));
#22622=DIRECTION('',(-2.44929359829471E-16,0.,-1.));
#22623=DIRECTION('',(-2.44929359829471E-16,0.,-1.));
#22624=DIRECTION('center_axis',(-2.44929359829471E-16,0.,-1.));
#22625=DIRECTION('ref_axis',(-1.,0.,2.44929359829471E-16));
#22626=DIRECTION('',(-2.44929359829471E-16,0.,-1.));
#22627=DIRECTION('',(-2.44929359829471E-16,0.,-1.));
#22628=DIRECTION('center_axis',(-2.44929359829471E-16,0.,-1.));
#22629=DIRECTION('ref_axis',(-1.,0.,2.44929359829471E-16));
#22630=DIRECTION('',(-2.44929359829471E-16,0.,-1.));
#22631=DIRECTION('',(-2.44929359829471E-16,0.,-1.));
#22632=DIRECTION('center_axis',(-2.44929359829471E-16,0.,-1.));
#22633=DIRECTION('ref_axis',(-1.,0.,2.44929359829471E-16));
#22634=DIRECTION('',(-2.44929359829471E-16,0.,-1.));
#22635=DIRECTION('',(-2.44929359829471E-16,0.,-1.));
#22636=DIRECTION('center_axis',(-2.44929359829471E-16,0.,-1.));
#22637=DIRECTION('ref_axis',(-1.,0.,2.44929359829471E-16));
#22638=DIRECTION('',(-2.44929359829471E-16,0.,-1.));
#22639=DIRECTION('',(-2.44929359829471E-16,0.,-1.));
#22640=DIRECTION('center_axis',(-2.44929359829471E-16,0.,-1.));
#22641=DIRECTION('ref_axis',(-1.,0.,2.44929359829471E-16));
#22642=DIRECTION('',(-2.44929359829471E-16,0.,-1.));
#22643=DIRECTION('',(-2.44929359829471E-16,0.,-1.));
#22644=DIRECTION('center_axis',(-2.44929359829471E-16,0.,-1.));
#22645=DIRECTION('ref_axis',(-1.,0.,2.44929359829471E-16));
#22646=DIRECTION('',(-2.44929359829471E-16,0.,-1.));
#22647=DIRECTION('',(-2.44929359829471E-16,0.,-1.));
#22648=DIRECTION('center_axis',(-2.44929359829471E-16,0.,-1.));
#22649=DIRECTION('ref_axis',(-1.,0.,2.44929359829471E-16));
#22650=DIRECTION('',(-2.44929359829471E-16,0.,-1.));
#22651=DIRECTION('',(-2.44929359829471E-16,0.,-1.));
#22652=DIRECTION('center_axis',(-2.44929359829471E-16,0.,-1.));
#22653=DIRECTION('ref_axis',(-1.,0.,2.44929359829471E-16));
#22654=DIRECTION('',(-2.44929359829471E-16,0.,-1.));
#22655=DIRECTION('',(-2.44929359829471E-16,0.,-1.));
#22656=DIRECTION('center_axis',(-2.44929359829471E-16,0.,-1.));
#22657=DIRECTION('ref_axis',(-1.,0.,2.44929359829471E-16));
#22658=DIRECTION('',(-2.44929359829471E-16,0.,-1.));
#22659=DIRECTION('',(-2.44929359829471E-16,0.,-1.));
#22660=DIRECTION('center_axis',(-2.44929359829471E-16,0.,-1.));
#22661=DIRECTION('ref_axis',(-1.,0.,2.44929359829471E-16));
#22662=DIRECTION('',(-2.44929359829471E-16,0.,-1.));
#22663=DIRECTION('',(-2.44929359829471E-16,0.,-1.));
#22664=DIRECTION('center_axis',(-2.44929359829471E-16,0.,-1.));
#22665=DIRECTION('ref_axis',(-1.,0.,2.44929359829471E-16));
#22666=DIRECTION('',(-2.44929359829471E-16,0.,-1.));
#22667=DIRECTION('',(-2.44929359829471E-16,0.,-1.));
#22668=DIRECTION('center_axis',(-2.44929359829471E-16,0.,-1.));
#22669=DIRECTION('ref_axis',(-1.,0.,2.44929359829471E-16));
#22670=DIRECTION('',(-2.44929359829471E-16,0.,-1.));
#22671=DIRECTION('',(-2.44929359829471E-16,0.,-1.));
#22672=DIRECTION('center_axis',(-2.44929359829471E-16,0.,-1.));
#22673=DIRECTION('ref_axis',(-1.,0.,2.44929359829471E-16));
#22674=DIRECTION('',(-2.44929359829471E-16,0.,-1.));
#22675=DIRECTION('',(-2.44929359829471E-16,0.,-1.));
#22676=DIRECTION('center_axis',(-2.44929359829471E-16,0.,-1.));
#22677=DIRECTION('ref_axis',(-1.,0.,2.44929359829471E-16));
#22678=DIRECTION('',(-2.44929359829471E-16,0.,-1.));
#22679=DIRECTION('',(-2.44929359829471E-16,0.,-1.));
#22680=DIRECTION('center_axis',(-2.44929359829471E-16,0.,-1.));
#22681=DIRECTION('ref_axis',(-1.,0.,2.44929359829471E-16));
#22682=DIRECTION('',(-2.44929359829471E-16,0.,-1.));
#22683=DIRECTION('',(-2.44929359829471E-16,0.,-1.));
#22684=DIRECTION('center_axis',(-2.44929359829471E-16,0.,-1.));
#22685=DIRECTION('ref_axis',(-1.,0.,2.44929359829471E-16));
#22686=DIRECTION('',(-2.44929359829471E-16,0.,-1.));
#22687=DIRECTION('',(-2.44929359829471E-16,0.,-1.));
#22688=DIRECTION('center_axis',(-2.44929359829471E-16,0.,-1.));
#22689=DIRECTION('ref_axis',(-1.,0.,2.44929359829471E-16));
#22690=DIRECTION('',(-2.44929359829471E-16,0.,-1.));
#22691=DIRECTION('',(-2.44929359829471E-16,0.,-1.));
#22692=DIRECTION('center_axis',(-2.44929359829471E-16,0.,-1.));
#22693=DIRECTION('ref_axis',(-1.,0.,2.44929359829471E-16));
#22694=DIRECTION('',(-2.44929359829471E-16,0.,-1.));
#22695=DIRECTION('',(-2.44929359829471E-16,0.,-1.));
#22696=DIRECTION('center_axis',(-2.44929359829471E-16,0.,-1.));
#22697=DIRECTION('ref_axis',(-1.,0.,2.44929359829471E-16));
#22698=DIRECTION('',(-2.44929359829471E-16,0.,-1.));
#22699=DIRECTION('',(-2.44929359829471E-16,0.,-1.));
#22700=DIRECTION('center_axis',(-2.44929359829471E-16,0.,-1.));
#22701=DIRECTION('ref_axis',(-1.,0.,2.44929359829471E-16));
#22702=DIRECTION('',(-2.44929359829471E-16,0.,-1.));
#22703=DIRECTION('',(-2.44929359829471E-16,0.,-1.));
#22704=DIRECTION('center_axis',(-2.44929359829471E-16,0.,-1.));
#22705=DIRECTION('ref_axis',(-1.,0.,2.44929359829471E-16));
#22706=DIRECTION('',(-2.44929359829471E-16,0.,-1.));
#22707=DIRECTION('',(-2.44929359829471E-16,0.,-1.));
#22708=DIRECTION('center_axis',(-2.44929359829471E-16,0.,-1.));
#22709=DIRECTION('ref_axis',(-1.,0.,2.44929359829471E-16));
#22710=DIRECTION('',(-2.44929359829471E-16,0.,-1.));
#22711=DIRECTION('',(-2.44929359829471E-16,0.,-1.));
#22712=DIRECTION('center_axis',(-2.44929359829471E-16,0.,-1.));
#22713=DIRECTION('ref_axis',(-1.,0.,2.44929359829471E-16));
#22714=DIRECTION('',(-2.44929359829471E-16,0.,-1.));
#22715=DIRECTION('',(-2.44929359829471E-16,0.,-1.));
#22716=DIRECTION('center_axis',(-2.44929359829471E-16,0.,-1.));
#22717=DIRECTION('ref_axis',(-1.,0.,2.44929359829471E-16));
#22718=DIRECTION('',(-2.44929359829471E-16,0.,-1.));
#22719=DIRECTION('',(-2.44929359829471E-16,0.,-1.));
#22720=DIRECTION('center_axis',(-2.44929359829471E-16,0.,-1.));
#22721=DIRECTION('ref_axis',(-1.,0.,2.44929359829471E-16));
#22722=DIRECTION('',(-2.44929359829471E-16,0.,-1.));
#22723=DIRECTION('',(-2.44929359829471E-16,0.,-1.));
#22724=DIRECTION('center_axis',(-2.44929359829471E-16,0.,-1.));
#22725=DIRECTION('ref_axis',(-1.,0.,2.44929359829471E-16));
#22726=DIRECTION('',(-2.44929359829471E-16,0.,-1.));
#22727=DIRECTION('',(-2.44929359829471E-16,0.,-1.));
#22728=DIRECTION('center_axis',(-2.44929359829471E-16,0.,-1.));
#22729=DIRECTION('ref_axis',(-1.,0.,2.44929359829471E-16));
#22730=DIRECTION('',(-2.44929359829471E-16,0.,-1.));
#22731=DIRECTION('',(-2.44929359829471E-16,0.,-1.));
#22732=DIRECTION('center_axis',(-2.44929359829471E-16,0.,-1.));
#22733=DIRECTION('ref_axis',(-1.,0.,2.44929359829471E-16));
#22734=DIRECTION('',(-2.44929359829471E-16,0.,-1.));
#22735=DIRECTION('',(-2.44929359829471E-16,0.,-1.));
#22736=DIRECTION('center_axis',(-2.44929359829471E-16,0.,-1.));
#22737=DIRECTION('ref_axis',(-1.,0.,2.44929359829471E-16));
#22738=DIRECTION('',(-2.44929359829471E-16,0.,-1.));
#22739=DIRECTION('',(-2.44929359829471E-16,0.,-1.));
#22740=DIRECTION('center_axis',(-2.44929359829471E-16,0.,-1.));
#22741=DIRECTION('ref_axis',(-1.,0.,2.44929359829471E-16));
#22742=DIRECTION('',(-2.44929359829471E-16,0.,-1.));
#22743=DIRECTION('',(-2.44929359829471E-16,0.,-1.));
#22744=DIRECTION('center_axis',(-2.44929359829471E-16,0.,-1.));
#22745=DIRECTION('ref_axis',(-1.,0.,2.44929359829471E-16));
#22746=DIRECTION('',(-2.44929359829471E-16,0.,-1.));
#22747=DIRECTION('',(-2.44929359829471E-16,0.,-1.));
#22748=DIRECTION('center_axis',(-2.44929359829471E-16,0.,-1.));
#22749=DIRECTION('ref_axis',(-1.,0.,2.44929359829471E-16));
#22750=DIRECTION('',(-2.44929359829471E-16,0.,-1.));
#22751=DIRECTION('',(-2.44929359829471E-16,0.,-1.));
#22752=DIRECTION('center_axis',(-2.44929359829471E-16,0.,-1.));
#22753=DIRECTION('ref_axis',(-1.,0.,2.44929359829471E-16));
#22754=DIRECTION('',(-2.44929359829471E-16,0.,-1.));
#22755=DIRECTION('',(-2.44929359829471E-16,0.,-1.));
#22756=DIRECTION('center_axis',(-2.44929359829471E-16,0.,-1.));
#22757=DIRECTION('ref_axis',(-1.,0.,2.44929359829471E-16));
#22758=DIRECTION('',(-2.44929359829471E-16,0.,-1.));
#22759=DIRECTION('',(-2.44929359829471E-16,0.,-1.));
#22760=DIRECTION('center_axis',(-2.44929359829471E-16,0.,-1.));
#22761=DIRECTION('ref_axis',(-1.,0.,2.44929359829471E-16));
#22762=DIRECTION('',(-2.44929359829471E-16,0.,-1.));
#22763=DIRECTION('',(-2.44929359829471E-16,0.,-1.));
#22764=DIRECTION('center_axis',(-2.44929359829471E-16,0.,-1.));
#22765=DIRECTION('ref_axis',(-1.,0.,2.44929359829471E-16));
#22766=DIRECTION('',(-2.44929359829471E-16,0.,-1.));
#22767=DIRECTION('',(-2.44929359829471E-16,0.,-1.));
#22768=DIRECTION('center_axis',(-2.44929359829471E-16,0.,-1.));
#22769=DIRECTION('ref_axis',(-1.,0.,2.44929359829471E-16));
#22770=DIRECTION('',(-2.44929359829471E-16,0.,-1.));
#22771=DIRECTION('',(-2.44929359829471E-16,0.,-1.));
#22772=DIRECTION('center_axis',(-2.44929359829471E-16,0.,-1.));
#22773=DIRECTION('ref_axis',(-1.,0.,2.44929359829471E-16));
#22774=DIRECTION('',(-2.44929359829471E-16,0.,-1.));
#22775=DIRECTION('',(-2.44929359829471E-16,0.,-1.));
#22776=DIRECTION('center_axis',(-2.44929359829471E-16,0.,-1.));
#22777=DIRECTION('ref_axis',(-1.,0.,2.44929359829471E-16));
#22778=DIRECTION('',(-2.44929359829471E-16,0.,-1.));
#22779=DIRECTION('',(-2.44929359829471E-16,0.,-1.));
#22780=DIRECTION('center_axis',(-2.44929359829471E-16,0.,-1.));
#22781=DIRECTION('ref_axis',(-1.,0.,2.44929359829471E-16));
#22782=DIRECTION('',(-2.44929359829471E-16,0.,-1.));
#22783=DIRECTION('',(-2.44929359829471E-16,0.,-1.));
#22784=DIRECTION('center_axis',(-2.44929359829471E-16,0.,-1.));
#22785=DIRECTION('ref_axis',(-1.,0.,2.44929359829471E-16));
#22786=DIRECTION('',(-2.44929359829471E-16,0.,-1.));
#22787=DIRECTION('',(-2.44929359829471E-16,0.,-1.));
#22788=DIRECTION('center_axis',(-2.44929359829471E-16,0.,-1.));
#22789=DIRECTION('ref_axis',(-1.,0.,2.44929359829471E-16));
#22790=DIRECTION('',(-2.44929359829471E-16,0.,-1.));
#22791=DIRECTION('',(-2.44929359829471E-16,0.,-1.));
#22792=DIRECTION('center_axis',(-2.44929359829471E-16,0.,-1.));
#22793=DIRECTION('ref_axis',(-1.,0.,2.44929359829471E-16));
#22794=DIRECTION('',(-2.44929359829471E-16,0.,-1.));
#22795=DIRECTION('',(-2.44929359829471E-16,0.,-1.));
#22796=DIRECTION('center_axis',(-2.44929359829471E-16,0.,-1.));
#22797=DIRECTION('ref_axis',(-1.,0.,2.44929359829471E-16));
#22798=DIRECTION('',(-2.44929359829471E-16,0.,-1.));
#22799=DIRECTION('',(-2.44929359829471E-16,0.,-1.));
#22800=DIRECTION('center_axis',(-2.44929359829471E-16,0.,-1.));
#22801=DIRECTION('ref_axis',(-1.,0.,2.44929359829471E-16));
#22802=DIRECTION('',(-2.44929359829471E-16,0.,-1.));
#22803=DIRECTION('',(-2.44929359829471E-16,0.,-1.));
#22804=DIRECTION('center_axis',(-2.44929359829471E-16,0.,-1.));
#22805=DIRECTION('ref_axis',(-1.,0.,2.44929359829471E-16));
#22806=DIRECTION('',(-2.44929359829471E-16,0.,-1.));
#22807=DIRECTION('',(-2.44929359829471E-16,0.,-1.));
#22808=DIRECTION('center_axis',(-2.44929359829471E-16,0.,-1.));
#22809=DIRECTION('ref_axis',(-1.,0.,2.44929359829471E-16));
#22810=DIRECTION('',(-2.44929359829471E-16,0.,-1.));
#22811=DIRECTION('',(-2.44929359829471E-16,0.,-1.));
#22812=DIRECTION('center_axis',(-2.44929359829471E-16,0.,-1.));
#22813=DIRECTION('ref_axis',(-1.,0.,2.44929359829471E-16));
#22814=DIRECTION('',(-2.44929359829471E-16,0.,-1.));
#22815=DIRECTION('',(-2.44929359829471E-16,0.,-1.));
#22816=DIRECTION('center_axis',(-2.44929359829471E-16,0.,-1.));
#22817=DIRECTION('ref_axis',(-1.,0.,2.44929359829471E-16));
#22818=DIRECTION('center_axis',(-2.44929359829471E-16,0.,-1.));
#22819=DIRECTION('ref_axis',(-1.,0.,2.44929359829471E-16));
#22820=DIRECTION('',(-2.44929359829471E-16,0.,-1.));
#22821=DIRECTION('',(-2.44929359829471E-16,0.,-1.));
#22822=DIRECTION('center_axis',(-2.44929359829471E-16,0.,-1.));
#22823=DIRECTION('ref_axis',(-1.,0.,2.44929359829471E-16));
#22824=DIRECTION('center_axis',(2.44929359829471E-16,0.,1.));
#22825=DIRECTION('ref_axis',(1.,0.,-2.44929359829471E-16));
#22826=DIRECTION('center_axis',(0.866025403784439,-0.499999999999999,-2.12115047744982E-16));
#22827=DIRECTION('ref_axis',(0.499999999999999,0.866025403784439,-1.22464679914735E-16));
#22828=DIRECTION('',(-2.44929359829471E-16,0.,-1.));
#22829=DIRECTION('center_axis',(-0.866025403784438,-0.500000000000001,2.12115047744981E-16));
#22830=DIRECTION('ref_axis',(0.500000000000001,-0.866025403784438,-1.22464679914736E-16));
#22831=DIRECTION('center_axis',(0.903898417468945,-0.427747181051069,-2.2139126074154E-16));
#22832=DIRECTION('ref_axis',(0.427747181051069,0.903898417468945,-1.04767843223699E-16));
#22833=DIRECTION('',(-2.44929359829471E-16,0.,-1.));
#22834=DIRECTION('center_axis',(-0.82238913392188,-0.568925401443124,2.01427244102199E-16));
#22835=DIRECTION('ref_axis',(0.568925401443124,-0.82238913392188,-1.39346534366189E-16));
#22836=DIRECTION('center_axis',(0.82238913392189,-0.56892540144311,-2.01427244102201E-16));
#22837=DIRECTION('ref_axis',(0.56892540144311,0.82238913392189,-1.39346534366186E-16));
#22838=DIRECTION('',(-2.44929359829471E-16,0.,-1.));
#22839=DIRECTION('center_axis',(-0.903898417468938,-0.427747181051084,2.21391260741539E-16));
#22840=DIRECTION('ref_axis',(0.427747181051084,-0.903898417468938,-1.04767843223703E-16));
#22841=DIRECTION('center_axis',(0.773280000057739,-0.634064698205714,-1.89398975383075E-16));
#22842=DIRECTION('ref_axis',(0.634064698205714,0.773280000057739,-1.55301060621992E-16));
#22843=DIRECTION('',(-2.44929359829471E-16,0.,-1.));
#22844=DIRECTION('center_axis',(-0.935756136317931,-0.352647775185578,2.2919415142485E-16));
#22845=DIRECTION('ref_axis',(0.352647775185578,-0.935756136317931,-8.63737938214907E-17));
#22846=DIRECTION('center_axis',(0.719024815375424,-0.694984399015069,-1.76110287731406E-16));
#22847=DIRECTION('ref_axis',(0.694984399015069,0.719024815375425,-1.7022208394223E-16));
#22848=DIRECTION('',(-2.44929359829471E-16,0.,-1.));
#22849=DIRECTION('center_axis',(-0.961386552468623,-0.275201556558999,2.35471792844802E-16));
#22850=DIRECTION('ref_axis',(0.275201556558999,-0.961386552468623,-6.74049410720695E-17));
#22851=DIRECTION('center_axis',(0.65998463917753,-0.751279093313334,-1.61649615171037E-16));
#22852=DIRECTION('ref_axis',(0.751279093313334,0.65998463917753,-1.840103073785E-16));
#22853=DIRECTION('',(-2.44929359829471E-16,0.,-1.));
#22854=DIRECTION('center_axis',(-0.980619099730252,-0.195923916978581,2.40182408333483E-16));
#22855=DIRECTION('ref_axis',(0.195923916978581,-0.980619099730252,-4.79875195608462E-17));
#22856=DIRECTION('center_axis',(0.59655237409571,-0.802574149197924,-1.46113191092013E-16));
#22857=DIRECTION('ref_axis',(0.802574149197924,0.59655237409571,-1.9657397257873E-16));
#22858=DIRECTION('',(-2.44929359829471E-16,0.,-1.));
#22859=DIRECTION('center_axis',(-0.99332578867394,-0.115342436055841,2.43294649522012E-16));
#22860=DIRECTION('ref_axis',(0.115342436055841,-0.99332578867394,-2.82507490243288E-17));
#22861=DIRECTION('center_axis',(0.529150151388497,-0.848528206535016,-1.29604407833252E-16));
#22862=DIRECTION('ref_axis',(0.848528206535016,0.529150151388497,-2.0782947042387E-16));
#22863=DIRECTION('',(-2.44929359829471E-16,0.,-1.));
#22864=DIRECTION('center_axis',(-0.999422058381221,-0.033993370251312,2.44787804958764E-16));
#22865=DIRECTION('ref_axis',(0.033993370251312,-0.999422058381221,-8.32597441410003E-18));
#22866=DIRECTION('center_axis',(0.458226521727423,-0.888835448654917,-1.12233128623583E-16));
#22867=DIRECTION('ref_axis',(0.888835448654917,0.458226521727423,-2.17701897432789E-16));
#22868=DIRECTION('',(-2.44929359829471E-16,0.,-1.));
#22869=DIRECTION('center_axis',(-0.998867339183009,0.047581915823728,2.44651937940661E-16));
#22870=DIRECTION('ref_axis',(-0.047581915823728,-0.998867339183009,1.16542081821655E-17));
#22871=DIRECTION('center_axis',(0.384253470166307,-0.923227637511546,-9.41149564600862E-17));
#22872=DIRECTION('ref_axis',(0.923227637511546,0.384253470166307,-2.26125554232578E-16));
#22873=DIRECTION('',(-2.44929359829471E-16,0.,-1.));
#22874=DIRECTION('center_axis',(-0.991665322644044,0.128840552099425,2.42887952640291E-16));
#22875=DIRECTION('ref_axis',(-0.128840552099425,-0.991665322644044,3.15568339457877E-17));
#22876=DIRECTION('center_axis',(0.307723275158594,-0.951475898762374,-7.53704647892225E-17));
#22877=DIRECTION('ref_axis',(0.951475898762374,0.307723275158594,-2.33044382777039E-16));
#22878=DIRECTION('',(-2.44929359829471E-16,0.,-1.));
#22879=DIRECTION('center_axis',(-0.977863936996144,0.209241775758096,2.39507588088791E-16));
#22880=DIRECTION('ref_axis',(-0.209241775758096,-0.977863936996144,5.1249454186012E-17));
#22881=DIRECTION('center_axis',(0.229145232525468,-0.973392244889412,-5.61243951104381E-17));
#22882=DIRECTION('ref_axis',(0.973392244889412,0.229145232525468,-2.38412339403735E-16));
#22883=DIRECTION('',(-2.44929359829471E-16,0.,-1.));
#22884=DIRECTION('center_axis',(-0.957555028183728,0.288250529921558,2.34533340054531E-16));
#22885=DIRECTION('ref_axis',(-0.288250529921558,-0.957555028183729,7.06010177641929E-17));
#22886=DIRECTION('center_axis',(0.149042266176187,-0.988830826225127,-3.6504826842067E-17));
#22887=DIRECTION('ref_axis',(0.988830826225127,0.149042266176187,-2.42193701246967E-16));
#22888=DIRECTION('',(-2.44929359829471E-16,0.,-1.));
#22889=DIRECTION('center_axis',(-0.930873748644209,0.365341024366383,2.27998311337486E-16));
#22890=DIRECTION('ref_axis',(-0.365341024366383,-0.930873748644209,8.94827432175012E-17));
#22891=DIRECTION('center_axis',(0.0679474481357467,-0.997688901557916,-1.66423249739346E-17));
#22892=DIRECTION('ref_axis',(0.997688901557916,0.0679474481357467,-2.44363303967548E-16));
#22893=DIRECTION('',(-2.44929359829471E-16,0.,-1.));
#22894=DIRECTION('center_axis',(-0.89799765789082,0.440000234571075,2.19945991475563E-16));
#22895=DIRECTION('ref_axis',(-0.440000234571075,-0.89799765789082,1.0776897577831E-16));
#22896=DIRECTION('center_axis',(-0.0135995489614973,-0.999907521857919,
3.33092882110907E-18));
#22897=DIRECTION('ref_axis',(0.999907521857919,-0.0135995489614973,-2.44906709217332E-16));
#22898=DIRECTION('',(-2.44929359829471E-16,0.,-1.));
#22899=DIRECTION('center_axis',(-0.859145540883353,0.511731315809626,2.10429967328904E-16));
#22900=DIRECTION('ref_axis',(-0.511731315809626,-0.859145540883353,1.25338023585944E-16));
#22901=DIRECTION('center_axis',(-0.0950560433041702,-0.995471922573086,
2.32820158344128E-17));
#22902=DIRECTION('ref_axis',(0.995471922573086,-0.0950560433041702,-2.43820300724038E-16));
#22903=DIRECTION('',(-2.44929359829471E-16,0.,-1.));
#22904=DIRECTION('center_axis',(-0.814575952050343,0.580056909571188,1.99513566468172E-16));
#22905=DIRECTION('ref_axis',(-0.580056909571188,-0.814575952050343,1.42072967525932E-16));
#22906=DIRECTION('center_axis',(-0.175879955361797,-0.984411621884836,4.30781648736008E-17));
#22907=DIRECTION('ref_axis',(0.984411621884836,-0.175879955361797,-2.41111308356944E-16));
#22908=DIRECTION('',(-2.44929359829471E-16,0.,-1.));
#22909=DIRECTION('center_axis',(-0.76458549465201,0.644522320302207,1.87269435740016E-16));
#22910=DIRECTION('ref_axis',(-0.644522320302207,-0.76458549465201,1.57862439307425E-16));
#22911=DIRECTION('center_axis',(-0.255533415334641,-0.966800224269427,6.25876358329519E-17));
#22912=DIRECTION('ref_axis',(0.966800224269427,-0.255533415334641,-2.36797760013299E-16));
#22913=DIRECTION('',(-2.44929359829471E-16,0.,-1.));
#22914=DIRECTION('center_axis',(-0.709506846934496,0.704698541330312,1.73779057814292E-16));
#22915=DIRECTION('ref_axis',(-0.704698541330313,-0.709506846934496,1.72601362600795E-16));
#22916=DIRECTION('center_axis',(-0.333486342588479,-0.942754930672314,8.16805964020677E-17));
#22917=DIRECTION('ref_axis',(0.942754930672314,-0.333486342588479,-2.30908361645647E-16));
#22918=DIRECTION('',(-2.44929359829471E-16,0.,-1.));
#22919=DIRECTION('center_axis',(-0.649706548211022,0.76018510983294,1.59132208930341E-16));
#22920=DIRECTION('ref_axis',(-0.76018510983294,-0.649706548211022,1.86191652303278E-16));
#22921=DIRECTION('center_axis',(-0.409219973253765,-0.912435758555192,1.00229986078478E-16));
#22922=DIRECTION('ref_axis',(0.912435758555192,-0.409219973253765,-2.23482306228441E-16));
#22923=DIRECTION('',(-2.44929359829471E-16,0.,-1.));
#22924=DIRECTION('center_axis',(-0.585582559603238,0.810612771851345,1.43426361450924E-16));
#22925=DIRECTION('ref_axis',(-0.810612771851345,-0.585582559603238,1.98542867279143E-16));
#22926=DIRECTION('center_axis',(-0.48223031251359,-0.876044477006188,1.18112361734319E-16));
#22927=DIRECTION('ref_axis',(0.876044477006188,-0.48223031251359,-2.14569012935269E-16));
#22928=DIRECTION('',(-2.44929359829471E-16,0.,-1.));
#22929=DIRECTION('center_axis',(-0.517561615675617,0.855645939614771,1.26766035199735E-16));
#22930=DIRECTION('ref_axis',(-0.855645939614771,-0.517561615675617,2.09572812230532E-16));
#22931=DIRECTION('center_axis',(-0.552031488606037,-0.833823263999873,1.35208719109986E-16));
#22932=DIRECTION('ref_axis',(0.833823263999873,-0.552031488606037,-2.04227798262409E-16));
#22933=DIRECTION('',(-2.44929359829471E-16,0.,-1.));
#22934=DIRECTION('center_axis',(-0.446096384587331,0.894984924821705,1.09262101899216E-16));
#22935=DIRECTION('ref_axis',(-0.894984924821705,-0.446096384587331,2.19208084693607E-16));
#22936=DIRECTION('center_axis',(-0.618158986220597,-0.786053094742794,1.51405284767845E-16));
#22937=DIRECTION('ref_axis',(0.786053094742794,-0.618158986220597,-1.92527481287327E-16));
#22938=DIRECTION('',(-2.44929359829471E-16,0.,-1.));
#22939=DIRECTION('center_axis',(-0.371662455660338,0.928367933016068,9.10310473375357E-17));
#22940=DIRECTION('ref_axis',(-0.928367933016068,-0.371662455660338,2.27384563519835E-16));
#22941=DIRECTION('center_axis',(-0.680172737770911,-0.733051871829834,1.66594273235688E-16));
#22942=DIRECTION('ref_axis',(0.733051871829834,-0.680172737770911,-1.79545925689076E-16));
#22943=DIRECTION('',(-2.44929359829471E-16,0.,-1.));
#22944=DIRECTION('center_axis',(-0.294755174410915,0.955572805786137,7.21941961748894E-17));
#22945=DIRECTION('ref_axis',(-0.955572805786137,-0.294755174410915,2.3404783559165E-16));
#22946=DIRECTION('center_axis',(-0.737660051971963,-0.675172309654892,1.80674604301267E-16));
#22947=DIRECTION('ref_axis',(0.675172309654892,-0.737660051971963,-1.65369521578358E-16));
#22948=DIRECTION('',(-2.44929359829471E-16,0.,-1.));
#22949=DIRECTION('center_axis',(-0.215886346106968,0.976418499192115,5.28769045479032E-17));
#22950=DIRECTION('ref_axis',(-0.976418499192115,-0.215886346106968,2.39153557932777E-16));
#22951=DIRECTION('center_axis',(-0.790238360232484,-0.612799587154786,1.93552575684433E-16));
#22952=DIRECTION('ref_axis',(0.612799587154786,-0.790238360232484,-1.50092610585586E-16));
#22953=DIRECTION('',(-2.44929359829471E-16,0.,-1.));
#22954=DIRECTION('center_axis',(-0.135580829788419,0.990766288583682,3.32077258452259E-17));
#22955=DIRECTION('ref_axis',(-0.990766288583682,-0.135580829788419,2.42667752803422E-16));
#22956=DIRECTION('center_axis',(-0.837557762585809,-0.54634878450698,2.05142486610346E-16));
#22957=DIRECTION('ref_axis',(0.54634878450698,-0.837557762585809,-1.33816858032904E-16));
#22958=DIRECTION('',(-2.44929359829471E-16,0.,-1.));
#22959=DIRECTION('center_axis',(-0.0543730454168903,0.998520691789656,1.33175552059377E-17));
#22960=DIRECTION('ref_axis',(-0.998520691789656,-0.0543730454168903,2.44567033816521E-16));
#22961=DIRECTION('center_axis',(-0.879303356216429,-0.476262120839485,2.15367208133995E-16));
#22962=DIRECTION('ref_axis',(0.476262120839484,-0.879303356216429,-1.16650576368241E-16));
#22963=DIRECTION('',(-2.44929359829471E-16,0.,-1.));
#22964=DIRECTION('center_axis',(0.0271965826009666,0.999630104536087,-6.66124156600408E-18));
#22965=DIRECTION('ref_axis',(-0.999630104536087,0.0271965826009666,2.44838761570291E-16));
#22966=DIRECTION('center_axis',(-0.915197331086271,-0.40300601133552,2.24158696420601E-16));
#22967=DIRECTION('ref_axis',(0.40300601133552,-0.915197331086272,-9.87080043638374E-17));
#22968=DIRECTION('',(-2.44929359829471E-16,0.,-1.));
#22969=DIRECTION('center_axis',(0.108585221848735,0.994087143864189,-2.65957088743518E-17));
#22970=DIRECTION('ref_axis',(-0.994087143864189,0.108585221848735,2.43481127761363E-16));
#22971=DIRECTION('center_axis',(-0.945000818714665,-0.327067963317431,2.31458445566109E-16));
#22972=DIRECTION('ref_axis',(0.327067963317431,-0.945000818714665,-8.01085468760672E-17));
#22973=DIRECTION('',(-2.44929359829471E-16,0.,-1.));
#22974=DIRECTION('center_axis',(0.1892512443604,0.981928697262709,-4.63531861281235E-17));
#22975=DIRECTION('ref_axis',(-0.981928697262709,0.1892512443604,2.40503167218741E-16));
#22976=DIRECTION('center_axis',(-0.968515481808673,-0.248953331965879,2.3721787694433E-16));
#22977=DIRECTION('ref_axis',(0.248953331965879,-0.968515481808673,-6.09759802258165E-17));
#22978=DIRECTION('',(-2.44929359829471E-16,0.,-1.));
#22979=DIRECTION('center_axis',(0.268657831065104,0.963235677187776,-6.58021905759501E-17));
#22980=DIRECTION('ref_axis',(-0.963235677187776,0.268657831065104,2.35924697778509E-16));
#22981=DIRECTION('center_axis',(-0.985584834165051,-0.169181957264503,2.41398662489681E-16));
#22982=DIRECTION('ref_axis',(0.169181957264503,-0.985584834165051,-4.14376284874917E-17));
#22983=DIRECTION('',(-2.44929359829471E-16,0.,-1.));
#22984=DIRECTION('center_axis',(0.346276544229492,0.938132482603859,-8.48132923020909E-17));
#22985=DIRECTION('ref_axis',(-0.93813248260386,0.346276544229492,2.29776188399395E-16));
#22986=DIRECTION('center_axis',(-0.996095282060112,-0.0882847045505903,
2.43972979764139E-16));
#22987=DIRECTION('ref_axis',(0.0882847045505904,-0.996095282060113,-2.16235161683101E-17));
#22988=DIRECTION('',(-2.44929359829471E-16,0.,-1.));
#22989=DIRECTION('center_axis',(0.421590844123641,0.906786171129178,-1.0325997556117E-16));
#22990=DIRECTION('ref_axis',(-0.906786171129178,0.421590844123641,2.22098556396887E-16));
#22991=DIRECTION('center_axis',(-0.999976880197217,-0.00679993169384408,
2.44923697110976E-16));
#22992=DIRECTION('ref_axis',(0.00679993169384408,-0.999976880197217,-1.66550291665736E-18));
#22993=DIRECTION('',(-2.44929359829471E-16,0.,-1.));
#22994=DIRECTION('center_axis',(0.49409952650774,0.86940534729482,-1.21019480719585E-16));
#22995=DIRECTION('ref_axis',(-0.86940534729482,0.49409952650774,2.12942895145239E-16));
#22996=DIRECTION('center_axis',(-0.997203797181181,0.074730093586415,2.44244487663104E-16));
#22997=DIRECTION('ref_axis',(-0.074730093586415,-0.997203797181181,1.83035939821171E-17));
#22998=DIRECTION('',(-2.44929359829471E-16,0.,-1.));
#22999=DIRECTION('center_axis',(0.563320058063614,0.826238774316,-1.37973621200621E-16));
#23000=DIRECTION('ref_axis',(-0.826238774316,0.563320058063614,2.02370134059504E-16));
#23001=DIRECTION('center_axis',(-0.98779448742195,0.155762802423454,2.41939871447338E-16));
#23002=DIRECTION('ref_axis',(-0.155762802423454,-0.98779448742195,3.8150883482821E-17));
#23003=DIRECTION('',(-2.44929359829471E-16,0.,-1.));
#23004=DIRECTION('center_axis',(0.628791787574343,0.777573718613909,-1.54009569996612E-16));
#23005=DIRECTION('ref_axis',(-0.777573718613909,0.628791787574343,1.90450633120326E-16));
#23006=DIRECTION('center_axis',(-0.971811568323544,0.235758935509419,2.38025185304359E-16));
#23007=DIRECTION('ref_axis',(-0.235758935509419,-0.971811568323544,5.77442851483994E-17));
#23008=DIRECTION('',(-2.44929359829471E-16,0.,-1.));
#23009=DIRECTION('center_axis',(0.690079011482106,0.723734038105076,-1.69020610514066E-16));
#23010=DIRECTION('ref_axis',(-0.723734038105076,0.690079011482105,1.77263714639874E-16));
#23011=DIRECTION('center_axis',(-0.949361403575568,0.314186131777054,2.32526480824571E-16));
#23012=DIRECTION('ref_axis',(-0.314186131777054,-0.949361403575568,7.69534081234516E-17));
#23013=DIRECTION('',(-2.44929359829471E-16,0.,-1.));
#23014=DIRECTION('center_axis',(0.746773873423478,0.665078026980365,-1.82906846754987E-16));
#23015=DIRECTION('ref_axis',(-0.665078026980365,0.746773873423478,1.62897135384948E-16));
#23016=DIRECTION('center_axis',(-0.920593395320402,0.390522471174776,2.25480350979065E-16));
#23017=DIRECTION('ref_axis',(-0.390522471174777,-0.920593395320402,9.56504188638609E-17));
#23018=DIRECTION('',(-2.44929359829471E-16,0.,-1.));
#23019=DIRECTION('center_axis',(0.798499078446234,0.60199603131625,-1.95575868108258E-16));
#23020=DIRECTION('ref_axis',(-0.60199603131625,0.798499078446233,1.47446502570171E-16));
#23021=DIRECTION('center_axis',(-0.885698989906598,0.464259947958503,2.16933686599432E-16));
#23022=DIRECTION('ref_axis',(-0.464259947958503,-0.885698989906598,1.13710891847939E-16));
#23023=DIRECTION('',(-2.44929359829471E-16,0.,-1.));
#23024=DIRECTION('center_axis',(0.844910403845004,0.53490785138608,-2.06943364327016E-16));
#23025=DIRECTION('ref_axis',(-0.53490785138608,0.844910403845004,1.3101463760775E-16));
#23026=DIRECTION('center_axis',(-0.844910403845013,0.534907851386066,2.06943364327019E-16));
#23027=DIRECTION('ref_axis',(-0.534907851386066,-0.844910403845013,1.31014637607747E-16));
#23028=DIRECTION('',(-2.44929359829471E-16,0.,-1.));
#23029=DIRECTION('center_axis',(0.88569898990659,0.464259947958518,-2.1693368659943E-16));
#23030=DIRECTION('ref_axis',(-0.464259947958518,0.88569898990659,1.13710891847943E-16));
#23031=DIRECTION('center_axis',(-0.798499078446244,0.601996031316237,1.95575868108261E-16));
#23032=DIRECTION('ref_axis',(-0.601996031316237,-0.798499078446243,1.47446502570168E-16));
#23033=DIRECTION('',(-2.44929359829471E-16,0.,-1.));
#23034=DIRECTION('center_axis',(0.920593395320395,0.390522471174792,-2.25480350979063E-16));
#23035=DIRECTION('ref_axis',(-0.390522471174792,0.920593395320395,9.56504188638647E-17));
#23036=DIRECTION('center_axis',(-0.746773873423489,0.665078026980353,1.82906846754989E-16));
#23037=DIRECTION('ref_axis',(-0.665078026980353,-0.746773873423489,1.62897135384945E-16));
#23038=DIRECTION('',(-2.44929359829471E-16,0.,-1.));
#23039=DIRECTION('center_axis',(0.949361403575562,0.31418613177707,-2.3252648082457E-16));
#23040=DIRECTION('ref_axis',(-0.31418613177707,0.949361403575562,7.69534081234555E-17));
#23041=DIRECTION('center_axis',(-0.690079011482118,0.723734038105065,1.69020610514069E-16));
#23042=DIRECTION('ref_axis',(-0.723734038105065,-0.690079011482118,1.77263714639871E-16));
#23043=DIRECTION('',(-2.44929359829471E-16,0.,-1.));
#23044=DIRECTION('center_axis',(0.97181156832354,0.235758935509435,-2.38025185304359E-16));
#23045=DIRECTION('ref_axis',(-0.235758935509435,0.97181156832354,5.77442851484034E-17));
#23046=DIRECTION('center_axis',(-0.628791787574355,0.777573718613899,1.54009569996615E-16));
#23047=DIRECTION('ref_axis',(-0.777573718613899,-0.628791787574355,1.90450633120323E-16));
#23048=DIRECTION('',(-2.44929359829471E-16,0.,-1.));
#23049=DIRECTION('center_axis',(0.987794487421947,0.15576280242347,-2.41939871447338E-16));
#23050=DIRECTION('ref_axis',(-0.15576280242347,0.987794487421947,3.81508834828249E-17));
#23051=DIRECTION('center_axis',(-0.563320058063628,0.826238774315991,1.37973621200625E-16));
#23052=DIRECTION('ref_axis',(-0.826238774315991,-0.563320058063628,2.02370134059502E-16));
#23053=DIRECTION('',(-2.44929359829471E-16,0.,-1.));
#23054=DIRECTION('center_axis',(0.99720379718118,0.0747300935864316,-2.44244487663104E-16));
#23055=DIRECTION('ref_axis',(-0.0747300935864316,0.99720379718118,1.83035939821211E-17));
#23056=DIRECTION('center_axis',(-0.494099526507755,0.869405347294812,1.21019480719589E-16));
#23057=DIRECTION('ref_axis',(-0.869405347294812,-0.494099526507755,2.12942895145237E-16));
#23058=DIRECTION('',(-2.44929359829471E-16,0.,-1.));
#23059=DIRECTION('center_axis',(0.999976880197217,-0.00679993169382737,
-2.44923697110976E-16));
#23060=DIRECTION('ref_axis',(0.00679993169382737,0.999976880197217,-1.66550291665327E-18));
#23061=DIRECTION('center_axis',(-0.421590844123656,0.906786171129171,1.03259975561173E-16));
#23062=DIRECTION('ref_axis',(-0.906786171129171,-0.421590844123656,2.22098556396885E-16));
#23063=DIRECTION('',(-2.44929359829471E-16,0.,-1.));
#23064=DIRECTION('center_axis',(0.996095282060114,-0.0882847045505736,-2.4397297976414E-16));
#23065=DIRECTION('ref_axis',(0.0882847045505736,0.996095282060114,-2.1623516168306E-17));
#23066=DIRECTION('center_axis',(-0.346276544229508,0.938132482603854,8.48132923020948E-17));
#23067=DIRECTION('ref_axis',(-0.938132482603854,-0.346276544229508,2.29776188399394E-16));
#23068=DIRECTION('',(-2.44929359829471E-16,0.,-1.));
#23069=DIRECTION('center_axis',(0.985584834165054,-0.169181957264487,-2.41398662489682E-16));
#23070=DIRECTION('ref_axis',(0.169181957264487,0.985584834165054,-4.14376284874876E-17));
#23071=DIRECTION('center_axis',(-0.26865783106512,0.963235677187772,6.58021905759539E-17));
#23072=DIRECTION('ref_axis',(-0.963235677187772,-0.26865783106512,2.35924697778508E-16));
#23073=DIRECTION('',(-2.44929359829471E-16,0.,-1.));
#23074=DIRECTION('center_axis',(0.968515481808677,-0.248953331965864,-2.37217876944331E-16));
#23075=DIRECTION('ref_axis',(0.248953331965864,0.968515481808677,-6.09759802258127E-17));
#23076=DIRECTION('center_axis',(-0.189251244360416,0.981928697262706,4.63531861281275E-17));
#23077=DIRECTION('ref_axis',(-0.981928697262706,-0.189251244360416,2.40503167218741E-16));
#23078=DIRECTION('',(-2.44929359829471E-16,0.,-1.));
#23079=DIRECTION('center_axis',(0.945000818714671,-0.327067963317415,-2.3145844556611E-16));
#23080=DIRECTION('ref_axis',(0.327067963317415,0.945000818714671,-8.01085468760634E-17));
#23081=DIRECTION('center_axis',(-0.108585221848752,0.994087143864187,2.65957088743558E-17));
#23082=DIRECTION('ref_axis',(-0.994087143864187,-0.108585221848752,2.43481127761362E-16));
#23083=DIRECTION('',(-2.44929359829471E-16,0.,-1.));
#23084=DIRECTION('center_axis',(0.915197331086278,-0.403006011335506,-2.24158696420602E-16));
#23085=DIRECTION('ref_axis',(0.403006011335506,0.915197331086278,-9.87080043638338E-17));
#23086=DIRECTION('center_axis',(-0.0271965826009838,0.999630104536087,6.66124156600828E-18));
#23087=DIRECTION('ref_axis',(-0.999630104536087,-0.0271965826009838,2.44838761570291E-16));
#23088=DIRECTION('',(-2.44929359829471E-16,0.,-1.));
#23089=DIRECTION('center_axis',(0.879303356216437,-0.476262120839469,-2.15367208133997E-16));
#23090=DIRECTION('ref_axis',(0.476262120839469,0.879303356216437,-1.16650576368237E-16));
#23091=DIRECTION('center_axis',(0.0543730454168737,0.998520691789657,-1.33175552059336E-17));
#23092=DIRECTION('ref_axis',(-0.998520691789657,0.0543730454168737,2.44567033816521E-16));
#23093=DIRECTION('',(-2.44929359829471E-16,0.,-1.));
#23094=DIRECTION('center_axis',(0.837557762585818,-0.546348784506966,-2.05142486610348E-16));
#23095=DIRECTION('ref_axis',(0.546348784506966,0.837557762585818,-1.33816858032901E-16));
#23096=DIRECTION('center_axis',(0.135580829788402,0.990766288583684,-3.32077258452218E-17));
#23097=DIRECTION('ref_axis',(-0.990766288583684,0.135580829788402,2.42667752803422E-16));
#23098=DIRECTION('',(-2.44929359829471E-16,0.,-1.));
#23099=DIRECTION('center_axis',(0.790238360232494,-0.612799587154772,-1.93552575684435E-16));
#23100=DIRECTION('ref_axis',(0.612799587154772,0.790238360232494,-1.50092610585582E-16));
#23101=DIRECTION('center_axis',(0.215886346106952,0.976418499192119,-5.28769045478992E-17));
#23102=DIRECTION('ref_axis',(-0.976418499192119,0.215886346106952,2.39153557932778E-16));
#23103=DIRECTION('',(-2.44929359829471E-16,0.,-1.));
#23104=DIRECTION('center_axis',(0.737660051971974,-0.675172309654879,-1.8067460430127E-16));
#23105=DIRECTION('ref_axis',(0.675172309654879,0.737660051971974,-1.65369521578355E-16));
#23106=DIRECTION('center_axis',(0.294755174410899,0.955572805786142,-7.21941961748855E-17));
#23107=DIRECTION('ref_axis',(-0.955572805786142,0.294755174410899,2.34047835591651E-16));
#23108=DIRECTION('',(-2.44929359829471E-16,0.,-1.));
#23109=DIRECTION('center_axis',(0.680172737770924,-0.733051871829822,-1.66594273235691E-16));
#23110=DIRECTION('ref_axis',(0.733051871829822,0.680172737770924,-1.79545925689074E-16));
#23111=DIRECTION('center_axis',(0.371662455660323,0.928367933016075,-9.10310473375319E-17));
#23112=DIRECTION('ref_axis',(-0.928367933016075,0.371662455660323,2.27384563519836E-16));
#23113=DIRECTION('',(-2.44929359829471E-16,0.,-1.));
#23114=DIRECTION('center_axis',(0.618158986220609,-0.786053094742784,-1.51405284767848E-16));
#23115=DIRECTION('ref_axis',(0.786053094742784,0.618158986220609,-1.92527481287324E-16));
#23116=DIRECTION('center_axis',(0.446096384587316,0.894984924821712,-1.09262101899213E-16));
#23117=DIRECTION('ref_axis',(-0.894984924821712,0.446096384587316,2.19208084693609E-16));
#23118=DIRECTION('',(-2.44929359829471E-16,0.,-1.));
#23119=DIRECTION('center_axis',(0.552031488606051,-0.833823263999864,-1.3520871910999E-16));
#23120=DIRECTION('ref_axis',(0.833823263999864,0.552031488606051,-2.04227798262407E-16));
#23121=DIRECTION('center_axis',(0.517561615675603,0.85564593961478,-1.26766035199732E-16));
#23122=DIRECTION('ref_axis',(-0.85564593961478,0.517561615675603,2.09572812230534E-16));
#23123=DIRECTION('',(-2.44929359829471E-16,0.,-1.));
#23124=DIRECTION('center_axis',(0.482230312513604,-0.87604447700618,-1.18112361734323E-16));
#23125=DIRECTION('ref_axis',(0.87604447700618,0.482230312513604,-2.14569012935267E-16));
#23126=DIRECTION('center_axis',(0.585582559603225,0.810612771851354,-1.43426361450921E-16));
#23127=DIRECTION('ref_axis',(-0.810612771851354,0.585582559603225,1.98542867279145E-16));
#23128=DIRECTION('',(-2.44929359829471E-16,0.,-1.));
#23129=DIRECTION('center_axis',(0.40921997325378,-0.912435758555185,-1.00229986078481E-16));
#23130=DIRECTION('ref_axis',(0.912435758555185,0.40921997325378,-2.23482306228439E-16));
#23131=DIRECTION('center_axis',(0.649706548211009,0.760185109832951,-1.59132208930338E-16));
#23132=DIRECTION('ref_axis',(-0.760185109832951,0.649706548211009,1.86191652303281E-16));
#23133=DIRECTION('',(-2.44929359829471E-16,0.,-1.));
#23134=DIRECTION('center_axis',(0.333486342588495,-0.942754930672308,-8.16805964020716E-17));
#23135=DIRECTION('ref_axis',(0.942754930672308,0.333486342588495,-2.30908361645646E-16));
#23136=DIRECTION('center_axis',(0.709506846934484,0.704698541330324,-1.73779057814289E-16));
#23137=DIRECTION('ref_axis',(-0.704698541330324,0.709506846934484,1.72601362600798E-16));
#23138=DIRECTION('',(-2.44929359829471E-16,0.,-1.));
#23139=DIRECTION('center_axis',(0.255533415334658,-0.966800224269422,-6.25876358329559E-17));
#23140=DIRECTION('ref_axis',(0.966800224269422,0.255533415334658,-2.36797760013298E-16));
#23141=DIRECTION('center_axis',(0.764585494652,0.64452232030222,-1.87269435740013E-16));
#23142=DIRECTION('ref_axis',(-0.64452232030222,0.764585494652,1.57862439307428E-16));
#23143=DIRECTION('',(-2.44929359829471E-16,0.,-1.));
#23144=DIRECTION('center_axis',(0.175879955361814,-0.984411621884833,-4.30781648736049E-17));
#23145=DIRECTION('ref_axis',(0.984411621884833,0.175879955361814,-2.41111308356943E-16));
#23146=DIRECTION('center_axis',(0.814575952050334,0.580056909571201,-1.9951356646817E-16));
#23147=DIRECTION('ref_axis',(-0.580056909571201,0.814575952050333,1.42072967525936E-16));
#23148=DIRECTION('',(-2.44929359829471E-16,0.,-1.));
#23149=DIRECTION('center_axis',(0.0950560433041868,-0.995471922573084,-2.32820158344169E-17));
#23150=DIRECTION('ref_axis',(0.995471922573084,0.0950560433041868,-2.43820300724038E-16));
#23151=DIRECTION('center_axis',(0.859145540883344,0.51173131580964,-2.10429967328902E-16));
#23152=DIRECTION('ref_axis',(-0.51173131580964,0.859145540883344,1.25338023585948E-16));
#23153=DIRECTION('',(-2.44929359829471E-16,0.,-1.));
#23154=DIRECTION('center_axis',(0.013599548961514,-0.999907521857918,-3.33092882111317E-18));
#23155=DIRECTION('ref_axis',(0.999907521857918,0.013599548961514,-2.44906709217332E-16));
#23156=DIRECTION('center_axis',(0.897997657890813,0.44000023457109,-2.19945991475561E-16));
#23157=DIRECTION('ref_axis',(-0.44000023457109,0.897997657890813,1.07768975778314E-16));
#23158=DIRECTION('',(-2.44929359829471E-16,0.,-1.));
#23159=DIRECTION('center_axis',(-0.0679474481357302,-0.997688901557917,
1.66423249739306E-17));
#23160=DIRECTION('ref_axis',(0.997688901557917,-0.0679474481357302,-2.44363303967548E-16));
#23161=DIRECTION('center_axis',(0.930873748644203,0.365341024366398,-2.27998311337484E-16));
#23162=DIRECTION('ref_axis',(-0.365341024366398,0.930873748644203,8.94827432175049E-17));
#23163=DIRECTION('',(-2.44929359829471E-16,0.,-1.));
#23164=DIRECTION('center_axis',(-0.149042266176171,-0.988830826225129,3.65048268420631E-17));
#23165=DIRECTION('ref_axis',(0.988830826225129,-0.149042266176171,-2.42193701246967E-16));
#23166=DIRECTION('center_axis',(0.957555028183724,0.288250529921574,-2.3453334005453E-16));
#23167=DIRECTION('ref_axis',(-0.288250529921574,0.957555028183724,7.06010177641968E-17));
#23168=DIRECTION('',(-2.44929359829471E-16,0.,-1.));
#23169=DIRECTION('center_axis',(-0.229145232525452,-0.973392244889416,5.61243951104342E-17));
#23170=DIRECTION('ref_axis',(0.973392244889416,-0.229145232525452,-2.38412339403736E-16));
#23171=DIRECTION('center_axis',(0.977863936996141,0.209241775758112,-2.39507588088791E-16));
#23172=DIRECTION('ref_axis',(-0.209241775758112,0.977863936996141,5.12494541860159E-17));
#23173=DIRECTION('',(-2.44929359829471E-16,0.,-1.));
#23174=DIRECTION('center_axis',(-0.307723275158579,-0.951475898762379,7.53704647892187E-17));
#23175=DIRECTION('ref_axis',(0.951475898762379,-0.307723275158579,-2.3304438277704E-16));
#23176=DIRECTION('center_axis',(0.991665322644042,0.128840552099442,-2.42887952640291E-16));
#23177=DIRECTION('ref_axis',(-0.128840552099442,0.991665322644042,3.15568339457918E-17));
#23178=DIRECTION('',(-2.44929359829471E-16,0.,-1.));
#23179=DIRECTION('center_axis',(-0.384253470166292,-0.923227637511553,9.41149564600824E-17));
#23180=DIRECTION('ref_axis',(0.923227637511553,-0.384253470166292,-2.26125554232579E-16));
#23181=DIRECTION('center_axis',(0.998867339183008,0.0475819158237449,-2.44651937940661E-16));
#23182=DIRECTION('ref_axis',(-0.0475819158237449,0.998867339183008,1.16542081821696E-17));
#23183=DIRECTION('',(-2.44929359829471E-16,0.,-1.));
#23184=DIRECTION('center_axis',(-0.458226521727408,-0.888835448654925,1.12233128623579E-16));
#23185=DIRECTION('ref_axis',(0.888835448654925,-0.458226521727408,-2.17701897432791E-16));
#23186=DIRECTION('center_axis',(0.999422058381222,-0.0339933702512953,-2.44787804958765E-16));
#23187=DIRECTION('ref_axis',(0.0339933702512953,0.999422058381222,-8.32597441409594E-18));
#23188=DIRECTION('',(-2.44929359829471E-16,0.,-1.));
#23189=DIRECTION('center_axis',(-0.529150151388483,-0.848528206535025,1.29604407833249E-16));
#23190=DIRECTION('ref_axis',(0.848528206535025,-0.529150151388483,-2.07829470423873E-16));
#23191=DIRECTION('center_axis',(0.993325788673942,-0.115342436055824,-2.43294649522013E-16));
#23192=DIRECTION('ref_axis',(0.115342436055824,0.993325788673942,-2.82507490243247E-17));
#23193=DIRECTION('',(-2.44929359829471E-16,0.,-1.));
#23194=DIRECTION('center_axis',(-0.596552374095697,-0.802574149197934,1.4611319109201E-16));
#23195=DIRECTION('ref_axis',(0.802574149197934,-0.596552374095697,-1.96573972578732E-16));
#23196=DIRECTION('center_axis',(0.980619099730256,-0.195923916978565,-2.40182408333483E-16));
#23197=DIRECTION('ref_axis',(0.195923916978565,0.980619099730256,-4.79875195608422E-17));
#23198=DIRECTION('',(-2.44929359829471E-16,0.,-1.));
#23199=DIRECTION('center_axis',(-0.659984639177518,-0.751279093313345,1.61649615171034E-16));
#23200=DIRECTION('ref_axis',(0.751279093313345,-0.659984639177518,-1.84010307378503E-16));
#23201=DIRECTION('center_axis',(0.961386552468627,-0.275201556558983,-2.35471792844803E-16));
#23202=DIRECTION('ref_axis',(0.275201556558983,0.961386552468627,-6.74049410720656E-17));
#23203=DIRECTION('',(-2.44929359829471E-16,0.,-1.));
#23204=DIRECTION('center_axis',(-0.719024815375413,-0.694984399015081,1.76110287731403E-16));
#23205=DIRECTION('ref_axis',(0.694984399015081,-0.719024815375413,-1.70222083942233E-16));
#23206=DIRECTION('center_axis',(0.935756136317937,-0.352647775185563,-2.29194151424851E-16));
#23207=DIRECTION('ref_axis',(0.352647775185563,0.935756136317937,-8.6373793821487E-17));
#23208=DIRECTION('',(-2.44929359829471E-16,0.,-1.));
#23209=DIRECTION('center_axis',(-0.773280000057729,-0.634064698205726,1.89398975383073E-16));
#23210=DIRECTION('ref_axis',(0.634064698205726,-0.773280000057729,-1.55301060621995E-16));
#23211=DIRECTION('center_axis',(0.,0.,1.));
#23212=DIRECTION('ref_axis',(1.,0.,0.));
#23213=DIRECTION('center_axis',(0.,0.,-1.));
#23214=DIRECTION('ref_axis',(1.,-2.57442419626753E-15,0.));
#23215=DIRECTION('center_axis',(0.,0.,1.));
#23216=DIRECTION('ref_axis',(1.,0.,0.));
#23217=DIRECTION('center_axis',(0.,0.,-1.));
#23218=DIRECTION('ref_axis',(1.,0.,0.));
#23219=DIRECTION('center_axis',(0.,-1.,0.));
#23220=DIRECTION('ref_axis',(-1.,0.,0.));
#23221=DIRECTION('center_axis',(0.,0.,-1.));
#23222=DIRECTION('ref_axis',(1.,0.,0.));
#23223=DIRECTION('center_axis',(0.,0.,-1.));
#23224=DIRECTION('ref_axis',(1.,0.,0.));
#23225=DIRECTION('center_axis',(0.,0.,-1.));
#23226=DIRECTION('ref_axis',(1.,0.,0.));
#23227=DIRECTION('center_axis',(0.,0.,1.));
#23228=DIRECTION('ref_axis',(1.,0.,0.));
#23229=DIRECTION('center_axis',(0.,0.,-1.));
#23230=DIRECTION('ref_axis',(-1.,0.,0.));
#23231=DIRECTION('center_axis',(0.,0.,1.));
#23232=DIRECTION('ref_axis',(1.,0.,0.));
#23233=DIRECTION('',(-0.0871557427476585,1.0673500138323E-17,0.996194698091746));
#23234=DIRECTION('center_axis',(0.,0.,1.));
#23235=DIRECTION('ref_axis',(1.,0.,0.));
#23236=DIRECTION('center_axis',(0.,0.,1.));
#23237=DIRECTION('ref_axis',(1.,0.,0.));
#23238=DIRECTION('',(0.,0.,-1.));
#23239=DIRECTION('center_axis',(0.,0.,1.));
#23240=DIRECTION('ref_axis',(1.,0.,0.));
#23241=DIRECTION('center_axis',(0.,0.,1.));
#23242=DIRECTION('ref_axis',(1.,0.,0.));
#23243=DIRECTION('',(-1.,0.,0.));
#23244=DIRECTION('center_axis',(0.,0.,-1.));
#23245=DIRECTION('ref_axis',(-1.,0.,0.));
#23246=DIRECTION('center_axis',(0.,0.,1.));
#23247=DIRECTION('ref_axis',(1.,0.,0.));
#23248=DIRECTION('',(1.,-1.25844895020639E-16,0.));
#23249=DIRECTION('center_axis',(0.,0.,1.));
#23250=DIRECTION('ref_axis',(1.,0.,0.));
#23251=DIRECTION('center_axis',(0.,1.,0.));
#23252=DIRECTION('ref_axis',(1.,0.,0.));
#23253=DIRECTION('',(-1.,0.,0.));
#23254=DIRECTION('center_axis',(-1.25844895020639E-16,-1.,0.));
#23255=DIRECTION('ref_axis',(-1.,1.25844895020639E-16,0.));
#23256=DIRECTION('',(1.,-1.25844895020639E-16,0.));
#23257=DIRECTION('center_axis',(0.,0.,1.));
#23258=DIRECTION('ref_axis',(1.,0.,0.));
#23259=DIRECTION('center_axis',(-1.22460635382238E-16,-1.,-2.46519032881566E-32));
#23260=DIRECTION('ref_axis',(0.,0.,1.));
#23261=DIRECTION('center_axis',(-1.22460635382238E-16,-1.,-2.46519032881566E-32));
#23262=DIRECTION('ref_axis',(-3.01888774004913E-48,-2.46519032881566E-32,
1.));
#23263=DIRECTION('center_axis',(-1.,1.22460635382238E-16,0.));
#23264=DIRECTION('ref_axis',(0.,0.,-1.));
#23265=DIRECTION('center_axis',(1.22460635382238E-16,1.,2.46519032881566E-32));
#23266=DIRECTION('ref_axis',(-3.01888774004913E-48,-2.46519032881566E-32,
1.));
#23267=DIRECTION('center_axis',(-1.22460635382238E-16,-1.,-2.46519032881566E-32));
#23268=DIRECTION('ref_axis',(-3.01888774004913E-48,-2.46519032881566E-32,
1.));
#23269=DIRECTION('center_axis',(0.,-1.,-2.46519032881566E-32));
#23270=DIRECTION('ref_axis',(-1.,0.,0.));
#23271=DIRECTION('center_axis',(0.,-1.,-2.46519032881566E-32));
#23272=DIRECTION('ref_axis',(-1.,0.,0.));
#23273=DIRECTION('',(-2.85991635543547E-21,0.707106781186549,0.707106781186546));
#23274=DIRECTION('center_axis',(-1.22460635382238E-16,-1.,-2.46519032881566E-32));
#23275=DIRECTION('ref_axis',(-3.01888774004913E-48,-2.46519032881566E-32,
1.));
#23276=DIRECTION('center_axis',(0.,-1.,-2.46519032881566E-32));
#23277=DIRECTION('ref_axis',(1.,0.,0.));
#23278=DIRECTION('center_axis',(0.,-1.,-2.46519032881566E-32));
#23279=DIRECTION('ref_axis',(1.,0.,0.));
#23280=DIRECTION('center_axis',(0.,-1.,-2.46519032881566E-32));
#23281=DIRECTION('ref_axis',(1.,0.,0.));
#23282=DIRECTION('',(0.81915204428899,0.573576436351049,1.00317192905352E-16));
#23283=DIRECTION('center_axis',(0.,-1.,-2.46519032881566E-32));
#23284=DIRECTION('ref_axis',(1.,0.,0.));
#23285=DIRECTION('center_axis',(0.,-1.,-2.46519032881566E-32));
#23286=DIRECTION('ref_axis',(1.,0.,0.));
#23287=DIRECTION('center_axis',(0.,1.,2.46519032881566E-32));
#23288=DIRECTION('ref_axis',(-1.,0.,0.));
#23289=DIRECTION('',(-0.819152044288993,-0.573576436351044,1.00317192905353E-16));
#23290=DIRECTION('center_axis',(-1.22460635382238E-16,-1.,-2.46519032881566E-32));
#23291=DIRECTION('ref_axis',(-3.01888774004913E-48,-2.46519032881566E-32,
1.));
#23292=DIRECTION('center_axis',(0.,-1.,-2.46519032881566E-32));
#23293=DIRECTION('ref_axis',(1.,0.,0.));
#23294=DIRECTION('center_axis',(0.,-1.,-2.46519032881566E-32));
#23295=DIRECTION('ref_axis',(1.,0.,0.));
#23296=DIRECTION('',(1.22460635382238E-16,1.,2.46519032881566E-32));
#23297=DIRECTION('center_axis',(0.,-1.,-2.46519032881566E-32));
#23298=DIRECTION('ref_axis',(1.,0.,0.));
#23299=DIRECTION('center_axis',(0.,-1.,-2.46519032881566E-32));
#23300=DIRECTION('ref_axis',(1.,0.,0.));
#23301=DIRECTION('center_axis',(0.,-1.,-2.46519032881566E-32));
#23302=DIRECTION('ref_axis',(1.,0.,0.));
#23303=DIRECTION('',(0.81915204428899,0.573576436351049,1.00317192905352E-16));
#23304=DIRECTION('center_axis',(0.,-1.,-2.46519032881566E-32));
#23305=DIRECTION('ref_axis',(1.,0.,0.));
#23306=DIRECTION('center_axis',(0.,-1.,-2.46519032881566E-32));
#23307=DIRECTION('ref_axis',(1.,0.,0.));
#23308=DIRECTION('center_axis',(0.,1.,2.46519032881566E-32));
#23309=DIRECTION('ref_axis',(-1.,0.,0.));
#23310=DIRECTION('',(-0.819152044288993,-0.573576436351044,1.00317192905353E-16));
#23311=DIRECTION('center_axis',(-1.22460635382238E-16,-1.,-2.46519032881566E-32));
#23312=DIRECTION('ref_axis',(-3.01888774004913E-48,-2.46519032881566E-32,
1.));
#23313=DIRECTION('center_axis',(0.,-1.,-2.46519032881566E-32));
#23314=DIRECTION('ref_axis',(1.,0.,0.));
#23315=DIRECTION('center_axis',(0.,-1.,-2.46519032881566E-32));
#23316=DIRECTION('ref_axis',(1.,0.,0.));
#23317=DIRECTION('',(1.22460635382238E-16,1.,2.46519032881566E-32));
#23318=DIRECTION('center_axis',(0.,-1.,-2.46519032881566E-32));
#23319=DIRECTION('ref_axis',(1.,0.,0.));
#23320=DIRECTION('center_axis',(0.,-1.,-2.46519032881566E-32));
#23321=DIRECTION('ref_axis',(1.,0.,0.));
#23322=DIRECTION('center_axis',(0.,-1.,-2.46519032881566E-32));
#23323=DIRECTION('ref_axis',(1.,0.,0.));
#23324=DIRECTION('',(0.81915204428899,0.573576436351049,1.00317192905352E-16));
#23325=DIRECTION('center_axis',(0.,-1.,-2.46519032881566E-32));
#23326=DIRECTION('ref_axis',(1.,0.,0.));
#23327=DIRECTION('center_axis',(0.,-1.,-2.46519032881566E-32));
#23328=DIRECTION('ref_axis',(1.,0.,0.));
#23329=DIRECTION('center_axis',(0.,1.,2.46519032881566E-32));
#23330=DIRECTION('ref_axis',(-1.,0.,0.));
#23331=DIRECTION('',(-0.819152044288993,-0.573576436351044,1.00317192905353E-16));
#23332=DIRECTION('center_axis',(-1.22460635382238E-16,-1.,-2.46519032881566E-32));
#23333=DIRECTION('ref_axis',(-3.01888774004913E-48,-2.46519032881566E-32,
1.));
#23334=DIRECTION('center_axis',(0.,-1.,-2.46519032881566E-32));
#23335=DIRECTION('ref_axis',(1.,0.,0.));
#23336=DIRECTION('center_axis',(0.,-1.,-2.46519032881566E-32));
#23337=DIRECTION('ref_axis',(1.,0.,0.));
#23338=DIRECTION('',(1.22460635382238E-16,1.,2.46519032881566E-32));
#23339=DIRECTION('center_axis',(0.,-1.,-2.46519032881566E-32));
#23340=DIRECTION('ref_axis',(1.,0.,0.));
#23341=DIRECTION('center_axis',(0.,-1.,-2.46519032881566E-32));
#23342=DIRECTION('ref_axis',(1.,0.,0.));
#23343=DIRECTION('center_axis',(0.,-1.,-2.46519032881566E-32));
#23344=DIRECTION('ref_axis',(1.,0.,0.));
#23345=DIRECTION('',(0.81915204428899,0.573576436351049,1.00317192905352E-16));
#23346=DIRECTION('center_axis',(0.,-1.,-2.46519032881566E-32));
#23347=DIRECTION('ref_axis',(1.,0.,0.));
#23348=DIRECTION('center_axis',(0.,-1.,-2.46519032881566E-32));
#23349=DIRECTION('ref_axis',(1.,0.,0.));
#23350=DIRECTION('center_axis',(0.,1.,2.46519032881566E-32));
#23351=DIRECTION('ref_axis',(-1.,0.,0.));
#23352=DIRECTION('',(-0.819152044288993,-0.573576436351044,1.00317192905353E-16));
#23353=DIRECTION('center_axis',(-1.22460635382238E-16,-1.,-2.46519032881566E-32));
#23354=DIRECTION('ref_axis',(-3.01888774004913E-48,-2.46519032881566E-32,
1.));
#23355=DIRECTION('center_axis',(0.,-1.,-2.46519032881566E-32));
#23356=DIRECTION('ref_axis',(1.,0.,0.));
#23357=DIRECTION('center_axis',(0.,-1.,-2.46519032881566E-32));
#23358=DIRECTION('ref_axis',(1.,0.,0.));
#23359=DIRECTION('',(1.22460635382238E-16,1.,2.46519032881566E-32));
#23360=DIRECTION('center_axis',(0.,-1.,-2.46519032881566E-32));
#23361=DIRECTION('ref_axis',(1.,0.,0.));
#23362=DIRECTION('center_axis',(0.,-1.,-2.46519032881566E-32));
#23363=DIRECTION('ref_axis',(1.,0.,0.));
#23364=DIRECTION('center_axis',(0.,-1.,-2.46519032881566E-32));
#23365=DIRECTION('ref_axis',(1.,0.,0.));
#23366=DIRECTION('',(0.81915204428899,0.573576436351049,1.00317192905352E-16));
#23367=DIRECTION('center_axis',(0.,-1.,-2.46519032881566E-32));
#23368=DIRECTION('ref_axis',(1.,0.,0.));
#23369=DIRECTION('center_axis',(0.,-1.,-2.46519032881566E-32));
#23370=DIRECTION('ref_axis',(1.,0.,0.));
#23371=DIRECTION('center_axis',(0.,1.,2.46519032881566E-32));
#23372=DIRECTION('ref_axis',(-1.,0.,0.));
#23373=DIRECTION('',(-0.819152044288993,-0.573576436351044,1.00317192905353E-16));
#23374=DIRECTION('center_axis',(-1.22460635382238E-16,-1.,-2.46519032881566E-32));
#23375=DIRECTION('ref_axis',(-3.01888774004913E-48,-2.46519032881566E-32,
1.));
#23376=DIRECTION('center_axis',(0.,-1.,-2.46519032881566E-32));
#23377=DIRECTION('ref_axis',(1.,0.,0.));
#23378=DIRECTION('center_axis',(0.,-1.,-2.46519032881566E-32));
#23379=DIRECTION('ref_axis',(1.,0.,0.));
#23380=DIRECTION('',(1.22460635382238E-16,1.,2.46519032881566E-32));
#23381=DIRECTION('center_axis',(0.,-1.,-2.46519032881566E-32));
#23382=DIRECTION('ref_axis',(1.,0.,0.));
#23383=DIRECTION('center_axis',(0.,-1.,-2.46519032881566E-32));
#23384=DIRECTION('ref_axis',(1.,0.,0.));
#23385=DIRECTION('center_axis',(0.,-1.,-2.46519032881566E-32));
#23386=DIRECTION('ref_axis',(1.,0.,0.));
#23387=DIRECTION('',(0.81915204428899,0.573576436351049,1.00317192905352E-16));
#23388=DIRECTION('center_axis',(0.,-1.,-2.46519032881566E-32));
#23389=DIRECTION('ref_axis',(1.,0.,0.));
#23390=DIRECTION('center_axis',(0.,-1.,-2.46519032881566E-32));
#23391=DIRECTION('ref_axis',(1.,0.,0.));
#23392=DIRECTION('center_axis',(0.,1.,2.46519032881566E-32));
#23393=DIRECTION('ref_axis',(-1.,0.,0.));
#23394=DIRECTION('',(-0.819152044288993,-0.573576436351044,1.00317192905353E-16));
#23395=DIRECTION('center_axis',(-1.22460635382238E-16,-1.,-2.46519032881566E-32));
#23396=DIRECTION('ref_axis',(-3.01888774004913E-48,-2.46519032881566E-32,
1.));
#23397=DIRECTION('center_axis',(0.,-1.,-2.46519032881566E-32));
#23398=DIRECTION('ref_axis',(1.,0.,0.));
#23399=DIRECTION('center_axis',(0.,-1.,-2.46519032881566E-32));
#23400=DIRECTION('ref_axis',(1.,0.,0.));
#23401=DIRECTION('',(1.22460635382238E-16,1.,2.46519032881566E-32));
#23402=DIRECTION('center_axis',(0.,-1.,-2.46519032881566E-32));
#23403=DIRECTION('ref_axis',(1.,0.,0.));
#23404=DIRECTION('center_axis',(0.,-1.,-2.46519032881566E-32));
#23405=DIRECTION('ref_axis',(1.,0.,0.));
#23406=DIRECTION('center_axis',(0.,-1.,-2.46519032881566E-32));
#23407=DIRECTION('ref_axis',(1.,0.,0.));
#23408=DIRECTION('',(0.81915204428899,0.573576436351049,1.00317192905352E-16));
#23409=DIRECTION('center_axis',(0.,-1.,-2.46519032881566E-32));
#23410=DIRECTION('ref_axis',(1.,0.,0.));
#23411=DIRECTION('center_axis',(0.,-1.,-2.46519032881566E-32));
#23412=DIRECTION('ref_axis',(1.,0.,0.));
#23413=DIRECTION('center_axis',(0.,1.,2.46519032881566E-32));
#23414=DIRECTION('ref_axis',(-1.,0.,0.));
#23415=DIRECTION('',(-0.819152044288993,-0.573576436351044,1.00317192905353E-16));
#23416=DIRECTION('center_axis',(-1.22460635382238E-16,-1.,-2.46519032881566E-32));
#23417=DIRECTION('ref_axis',(-3.01888774004913E-48,-2.46519032881566E-32,
1.));
#23418=DIRECTION('center_axis',(0.,-1.,-2.46519032881566E-32));
#23419=DIRECTION('ref_axis',(1.,0.,0.));
#23420=DIRECTION('center_axis',(0.,-1.,-2.46519032881566E-32));
#23421=DIRECTION('ref_axis',(1.,0.,0.));
#23422=DIRECTION('',(1.22460635382238E-16,1.,2.46519032881566E-32));
#23423=DIRECTION('center_axis',(0.,-1.,-2.46519032881566E-32));
#23424=DIRECTION('ref_axis',(1.,0.,0.));
#23425=DIRECTION('center_axis',(0.,-1.,-2.46519032881566E-32));
#23426=DIRECTION('ref_axis',(1.,0.,0.));
#23427=DIRECTION('center_axis',(0.,-1.,-2.46519032881566E-32));
#23428=DIRECTION('ref_axis',(1.,0.,0.));
#23429=DIRECTION('',(0.81915204428899,0.573576436351049,1.00317192905352E-16));
#23430=DIRECTION('center_axis',(0.,-1.,-2.46519032881566E-32));
#23431=DIRECTION('ref_axis',(1.,0.,0.));
#23432=DIRECTION('center_axis',(0.,-1.,-2.46519032881566E-32));
#23433=DIRECTION('ref_axis',(1.,0.,0.));
#23434=DIRECTION('center_axis',(0.,1.,2.46519032881566E-32));
#23435=DIRECTION('ref_axis',(-1.,0.,0.));
#23436=DIRECTION('',(-0.819152044288993,-0.573576436351044,1.00317192905353E-16));
#23437=DIRECTION('center_axis',(-1.22460635382238E-16,-1.,-2.46519032881566E-32));
#23438=DIRECTION('ref_axis',(-3.01888774004913E-48,-2.46519032881566E-32,
1.));
#23439=DIRECTION('center_axis',(0.,-1.,-2.46519032881566E-32));
#23440=DIRECTION('ref_axis',(1.,0.,0.));
#23441=DIRECTION('center_axis',(0.,-1.,-2.46519032881566E-32));
#23442=DIRECTION('ref_axis',(1.,0.,0.));
#23443=DIRECTION('',(1.22460635382238E-16,1.,2.46519032881566E-32));
#23444=DIRECTION('center_axis',(0.,-1.,-2.46519032881566E-32));
#23445=DIRECTION('ref_axis',(1.,0.,0.));
#23446=DIRECTION('center_axis',(0.,-1.,-2.46519032881566E-32));
#23447=DIRECTION('ref_axis',(1.,0.,0.));
#23448=DIRECTION('center_axis',(0.,-1.,-2.46519032881566E-32));
#23449=DIRECTION('ref_axis',(1.,0.,0.));
#23450=DIRECTION('',(0.81915204428899,0.573576436351049,1.00317192905352E-16));
#23451=DIRECTION('center_axis',(0.,-1.,-2.46519032881566E-32));
#23452=DIRECTION('ref_axis',(1.,0.,0.));
#23453=DIRECTION('center_axis',(0.,-1.,-2.46519032881566E-32));
#23454=DIRECTION('ref_axis',(1.,0.,0.));
#23455=DIRECTION('center_axis',(0.,1.,2.46519032881566E-32));
#23456=DIRECTION('ref_axis',(-1.,0.,0.));
#23457=DIRECTION('',(-0.819152044288993,-0.573576436351044,1.00317192905353E-16));
#23458=DIRECTION('center_axis',(-1.22460635382238E-16,-1.,-2.46519032881566E-32));
#23459=DIRECTION('ref_axis',(-3.01888774004913E-48,-2.46519032881566E-32,
1.));
#23460=DIRECTION('center_axis',(0.,-1.,-2.46519032881566E-32));
#23461=DIRECTION('ref_axis',(1.,0.,0.));
#23462=DIRECTION('center_axis',(0.,-1.,-2.46519032881566E-32));
#23463=DIRECTION('ref_axis',(1.,0.,0.));
#23464=DIRECTION('',(1.22460635382238E-16,1.,2.46519032881566E-32));
#23465=DIRECTION('center_axis',(0.,-1.,-2.46519032881566E-32));
#23466=DIRECTION('ref_axis',(1.,0.,0.));
#23467=DIRECTION('center_axis',(0.,-1.,-2.46519032881566E-32));
#23468=DIRECTION('ref_axis',(1.,0.,0.));
#23469=DIRECTION('center_axis',(0.,-1.,-2.46519032881566E-32));
#23470=DIRECTION('ref_axis',(1.,0.,0.));
#23471=DIRECTION('',(0.81915204428899,0.573576436351049,1.00317192905352E-16));
#23472=DIRECTION('center_axis',(0.,-1.,-2.46519032881566E-32));
#23473=DIRECTION('ref_axis',(1.,0.,0.));
#23474=DIRECTION('center_axis',(0.,-1.,-2.46519032881566E-32));
#23475=DIRECTION('ref_axis',(1.,0.,0.));
#23476=DIRECTION('center_axis',(0.,1.,2.46519032881566E-32));
#23477=DIRECTION('ref_axis',(-1.,0.,0.));
#23478=DIRECTION('',(-0.819152044288993,-0.573576436351044,1.00317192905353E-16));
#23479=DIRECTION('center_axis',(-1.22460635382238E-16,-1.,-2.46519032881566E-32));
#23480=DIRECTION('ref_axis',(-3.01888774004913E-48,-2.46519032881566E-32,
1.));
#23481=DIRECTION('center_axis',(0.,-1.,-2.46519032881566E-32));
#23482=DIRECTION('ref_axis',(1.,0.,0.));
#23483=DIRECTION('center_axis',(0.,-1.,-2.46519032881566E-32));
#23484=DIRECTION('ref_axis',(1.,0.,0.));
#23485=DIRECTION('',(1.22460635382238E-16,1.,2.46519032881566E-32));
#23486=DIRECTION('center_axis',(0.,-1.,-2.46519032881566E-32));
#23487=DIRECTION('ref_axis',(1.,0.,0.));
#23488=DIRECTION('center_axis',(0.,-1.,-2.46519032881566E-32));
#23489=DIRECTION('ref_axis',(1.,0.,0.));
#23490=DIRECTION('center_axis',(0.,-1.,-2.46519032881566E-32));
#23491=DIRECTION('ref_axis',(1.,0.,0.));
#23492=DIRECTION('',(0.81915204428899,0.573576436351049,1.00317192905352E-16));
#23493=DIRECTION('center_axis',(0.,-1.,-2.46519032881566E-32));
#23494=DIRECTION('ref_axis',(1.,0.,0.));
#23495=DIRECTION('center_axis',(0.,-1.,-2.46519032881566E-32));
#23496=DIRECTION('ref_axis',(1.,0.,0.));
#23497=DIRECTION('center_axis',(0.,1.,2.46519032881566E-32));
#23498=DIRECTION('ref_axis',(-1.,0.,0.));
#23499=DIRECTION('',(-0.819152044288993,-0.573576436351044,1.00317192905353E-16));
#23500=DIRECTION('center_axis',(-1.22460635382238E-16,-1.,-2.46519032881566E-32));
#23501=DIRECTION('ref_axis',(-3.01888774004913E-48,-2.46519032881566E-32,
1.));
#23502=DIRECTION('center_axis',(0.,-1.,-2.46519032881566E-32));
#23503=DIRECTION('ref_axis',(1.,0.,0.));
#23504=DIRECTION('center_axis',(0.,-1.,-2.46519032881566E-32));
#23505=DIRECTION('ref_axis',(1.,0.,0.));
#23506=DIRECTION('',(1.22460635382238E-16,1.,2.46519032881566E-32));
#23507=DIRECTION('center_axis',(0.,-1.,-2.46519032881566E-32));
#23508=DIRECTION('ref_axis',(1.,0.,0.));
#23509=DIRECTION('center_axis',(0.,-1.,-2.46519032881566E-32));
#23510=DIRECTION('ref_axis',(1.,0.,0.));
#23511=DIRECTION('center_axis',(0.,-1.,-2.46519032881566E-32));
#23512=DIRECTION('ref_axis',(1.,0.,0.));
#23513=DIRECTION('',(0.81915204428899,0.573576436351049,1.00317192905352E-16));
#23514=DIRECTION('center_axis',(0.,-1.,-2.46519032881566E-32));
#23515=DIRECTION('ref_axis',(1.,0.,0.));
#23516=DIRECTION('center_axis',(0.,-1.,-2.46519032881566E-32));
#23517=DIRECTION('ref_axis',(1.,0.,0.));
#23518=DIRECTION('center_axis',(0.,1.,2.46519032881566E-32));
#23519=DIRECTION('ref_axis',(-1.,0.,0.));
#23520=DIRECTION('',(-0.819152044288993,-0.573576436351044,1.00317192905353E-16));
#23521=DIRECTION('center_axis',(-1.22460635382238E-16,-1.,-2.46519032881566E-32));
#23522=DIRECTION('ref_axis',(-3.01888774004913E-48,-2.46519032881566E-32,
1.));
#23523=DIRECTION('center_axis',(0.,-1.,-2.46519032881566E-32));
#23524=DIRECTION('ref_axis',(1.,0.,0.));
#23525=DIRECTION('center_axis',(0.,-1.,-2.46519032881566E-32));
#23526=DIRECTION('ref_axis',(1.,0.,0.));
#23527=DIRECTION('',(1.22460635382238E-16,1.,2.46519032881566E-32));
#23528=DIRECTION('center_axis',(0.,-1.,-2.46519032881566E-32));
#23529=DIRECTION('ref_axis',(1.,0.,0.));
#23530=DIRECTION('center_axis',(0.,-1.,-2.46519032881566E-32));
#23531=DIRECTION('ref_axis',(1.,0.,0.));
#23532=DIRECTION('center_axis',(0.,-1.,-2.46519032881566E-32));
#23533=DIRECTION('ref_axis',(1.,0.,0.));
#23534=DIRECTION('',(0.81915204428899,0.573576436351049,1.00317192905352E-16));
#23535=DIRECTION('center_axis',(0.,-1.,-2.46519032881566E-32));
#23536=DIRECTION('ref_axis',(1.,0.,0.));
#23537=DIRECTION('center_axis',(0.,-1.,-2.46519032881566E-32));
#23538=DIRECTION('ref_axis',(1.,0.,0.));
#23539=DIRECTION('center_axis',(0.,1.,2.46519032881566E-32));
#23540=DIRECTION('ref_axis',(-1.,0.,0.));
#23541=DIRECTION('',(-0.819152044288993,-0.573576436351044,1.00317192905353E-16));
#23542=DIRECTION('center_axis',(-1.22460635382238E-16,-1.,-2.46519032881566E-32));
#23543=DIRECTION('ref_axis',(-3.01888774004913E-48,-2.46519032881566E-32,
1.));
#23544=DIRECTION('',(1.22460635382238E-16,1.,2.46519032881566E-32));
#23545=DIRECTION('center_axis',(-1.22460635382238E-16,-1.,-2.46519032881566E-32));
#23546=DIRECTION('ref_axis',(-3.01888774004913E-48,-2.46519032881566E-32,
1.));
#23547=DIRECTION('center_axis',(-1.22460635382238E-16,-1.,-2.46519032881566E-32));
#23548=DIRECTION('ref_axis',(-3.01888774004913E-48,-2.46519032881566E-32,
1.));
#23549=DIRECTION('center_axis',(-1.22460635382238E-16,-1.,-2.46519032881566E-32));
#23550=DIRECTION('ref_axis',(-3.01888774004913E-48,-2.46519032881566E-32,
1.));
#23551=DIRECTION('center_axis',(-1.22460635382238E-16,-1.,-2.46519032881566E-32));
#23552=DIRECTION('ref_axis',(-3.01888774004913E-48,-2.46519032881566E-32,
1.));
#23553=DIRECTION('center_axis',(-1.22460635382238E-16,-1.,-2.46519032881566E-32));
#23554=DIRECTION('ref_axis',(-3.01888774004913E-48,-2.46519032881566E-32,
1.));
#23555=DIRECTION('center_axis',(-1.22460635382238E-16,-1.,-2.46519032881566E-32));
#23556=DIRECTION('ref_axis',(-3.01888774004913E-48,-2.46519032881566E-32,
1.));
#23557=DIRECTION('center_axis',(-1.22460635382238E-16,-1.,-2.46519032881566E-32));
#23558=DIRECTION('ref_axis',(-3.01888774004913E-48,-2.46519032881566E-32,
1.));
#23559=DIRECTION('center_axis',(-1.22460635382238E-16,-1.,-2.46519032881566E-32));
#23560=DIRECTION('ref_axis',(-3.01888774004913E-48,-2.46519032881566E-32,
1.));
#23561=DIRECTION('center_axis',(-1.22460635382238E-16,-1.,-2.46519032881566E-32));
#23562=DIRECTION('ref_axis',(-3.01888774004913E-48,-2.46519032881566E-32,
1.));
#23563=DIRECTION('center_axis',(-1.22460635382238E-16,-1.,-2.46519032881566E-32));
#23564=DIRECTION('ref_axis',(-3.01888774004913E-48,-2.46519032881566E-32,
1.));
#23565=DIRECTION('center_axis',(-1.22460635382238E-16,-1.,-2.46519032881566E-32));
#23566=DIRECTION('ref_axis',(-3.01888774004913E-48,-2.46519032881566E-32,
1.));
#23567=DIRECTION('center_axis',(-1.22460635382238E-16,-1.,-2.46519032881566E-32));
#23568=DIRECTION('ref_axis',(-3.01888774004913E-48,-2.46519032881566E-32,
1.));
#23569=DIRECTION('center_axis',(-1.22460635382238E-16,-1.,-2.46519032881566E-32));
#23570=DIRECTION('ref_axis',(-3.01888774004913E-48,-2.46519032881566E-32,
1.));
#23571=DIRECTION('center_axis',(-1.22460635382238E-16,-1.,-2.46519032881566E-32));
#23572=DIRECTION('ref_axis',(-3.01888774004913E-48,-2.46519032881566E-32,
1.));
#23573=DIRECTION('center_axis',(-1.22460635382238E-16,-1.,-2.46519032881566E-32));
#23574=DIRECTION('ref_axis',(-3.01888774004913E-48,-2.46519032881566E-32,
1.));
#23575=DIRECTION('center_axis',(-1.22460635382238E-16,-1.,-2.46519032881566E-32));
#23576=DIRECTION('ref_axis',(-3.01888774004913E-48,-2.46519032881566E-32,
1.));
#23577=DIRECTION('center_axis',(-1.22460635382238E-16,-1.,-2.46519032881566E-32));
#23578=DIRECTION('ref_axis',(-3.01888774004913E-48,-2.46519032881566E-32,
1.));
#23579=DIRECTION('center_axis',(-1.22460635382238E-16,-1.,-2.46519032881566E-32));
#23580=DIRECTION('ref_axis',(-3.01888774004913E-48,-2.46519032881566E-32,
1.));
#23581=DIRECTION('center_axis',(-1.22460635382238E-16,-1.,-2.46519032881566E-32));
#23582=DIRECTION('ref_axis',(-3.01888774004913E-48,-2.46519032881566E-32,
1.));
#23583=DIRECTION('center_axis',(-1.22460635382238E-16,-1.,-2.46519032881566E-32));
#23584=DIRECTION('ref_axis',(-3.01888774004913E-48,-2.46519032881566E-32,
1.));
#23585=DIRECTION('center_axis',(-1.22460635382238E-16,-1.,-2.46519032881566E-32));
#23586=DIRECTION('ref_axis',(-3.01888774004913E-48,-2.46519032881566E-32,
1.));
#23587=DIRECTION('center_axis',(-1.22460635382238E-16,-1.,-2.46519032881566E-32));
#23588=DIRECTION('ref_axis',(-3.01888774004913E-48,-2.46519032881566E-32,
1.));
#23589=DIRECTION('center_axis',(-1.22460635382238E-16,-1.,-2.46519032881566E-32));
#23590=DIRECTION('ref_axis',(-3.01888774004913E-48,-2.46519032881566E-32,
1.));
#23591=DIRECTION('center_axis',(-1.22460635382238E-16,-1.,-2.46519032881566E-32));
#23592=DIRECTION('ref_axis',(-3.01888774004913E-48,-2.46519032881566E-32,
1.));
#23593=DIRECTION('center_axis',(-1.22460635382238E-16,-1.,-2.46519032881566E-32));
#23594=DIRECTION('ref_axis',(-3.01888774004913E-48,-2.46519032881566E-32,
1.));
#23595=DIRECTION('center_axis',(-1.22460635382238E-16,-1.,-2.46519032881566E-32));
#23596=DIRECTION('ref_axis',(-3.01888774004913E-48,-2.46519032881566E-32,
1.));
#23597=DIRECTION('center_axis',(-1.22460635382238E-16,-1.,-2.46519032881566E-32));
#23598=DIRECTION('ref_axis',(-3.01888774004913E-48,-2.46519032881566E-32,
1.));
#23599=DIRECTION('center_axis',(-1.22460635382238E-16,-1.,-2.46519032881566E-32));
#23600=DIRECTION('ref_axis',(-3.01888774004913E-48,-2.46519032881566E-32,
1.));
#23601=DIRECTION('center_axis',(-1.22460635382238E-16,-1.,-2.46519032881566E-32));
#23602=DIRECTION('ref_axis',(-3.01888774004913E-48,-2.46519032881566E-32,
1.));
#23603=DIRECTION('center_axis',(-1.22460635382238E-16,-1.,-2.46519032881566E-32));
#23604=DIRECTION('ref_axis',(-3.01888774004913E-48,-2.46519032881566E-32,
1.));
#23605=DIRECTION('center_axis',(-1.22460635382238E-16,-1.,-2.46519032881566E-32));
#23606=DIRECTION('ref_axis',(-3.01888774004913E-48,-2.46519032881566E-32,
1.));
#23607=DIRECTION('center_axis',(-1.22460635382238E-16,-1.,-2.46519032881566E-32));
#23608=DIRECTION('ref_axis',(-3.01888774004913E-48,-2.46519032881566E-32,
1.));
#23609=DIRECTION('center_axis',(-1.22460635382238E-16,-1.,-2.46519032881566E-32));
#23610=DIRECTION('ref_axis',(-3.01888774004913E-48,-2.46519032881566E-32,
1.));
#23611=DIRECTION('center_axis',(-1.22460635382238E-16,-1.,-2.46519032881566E-32));
#23612=DIRECTION('ref_axis',(-3.01888774004913E-48,-2.46519032881566E-32,
1.));
#23613=DIRECTION('center_axis',(-1.22460635382238E-16,-1.,-2.46519032881566E-32));
#23614=DIRECTION('ref_axis',(-3.01888774004913E-48,-2.46519032881566E-32,
1.));
#23615=DIRECTION('center_axis',(-1.22460635382238E-16,-1.,-2.46519032881566E-32));
#23616=DIRECTION('ref_axis',(-3.01888774004913E-48,-2.46519032881566E-32,
1.));
#23617=DIRECTION('center_axis',(-1.22460635382238E-16,-1.,-2.46519032881566E-32));
#23618=DIRECTION('ref_axis',(-3.01888774004913E-48,-2.46519032881566E-32,
1.));
#23619=DIRECTION('center_axis',(-1.22460635382238E-16,-1.,-2.46519032881566E-32));
#23620=DIRECTION('ref_axis',(-3.01888774004913E-48,-2.46519032881566E-32,
1.));
#23621=DIRECTION('center_axis',(-1.22460635382238E-16,-1.,-2.46519032881566E-32));
#23622=DIRECTION('ref_axis',(-3.01888774004913E-48,-2.46519032881566E-32,
1.));
#23623=DIRECTION('center_axis',(-1.22460635382238E-16,-1.,-2.46519032881566E-32));
#23624=DIRECTION('ref_axis',(-3.01888774004913E-48,-2.46519032881566E-32,
1.));
#23625=DIRECTION('center_axis',(-1.22460635382238E-16,-1.,-2.46519032881566E-32));
#23626=DIRECTION('ref_axis',(-3.01888774004913E-48,-2.46519032881566E-32,
1.));
#23627=DIRECTION('',(-2.85991635595236E-21,0.707106781186547,0.707106781186548));
#23628=DIRECTION('center_axis',(-1.22460635382238E-16,-1.,-2.46519032881566E-32));
#23629=DIRECTION('ref_axis',(-3.01888774004913E-48,-2.46519032881566E-32,
1.));
#23630=DIRECTION('center_axis',(-1.22460635382238E-16,-1.,-2.46519032881566E-32));
#23631=DIRECTION('ref_axis',(-3.01888774004913E-48,-2.46519032881566E-32,
1.));
#23632=DIRECTION('center_axis',(-1.22460635382238E-16,-1.,-2.46519032881566E-32));
#23633=DIRECTION('ref_axis',(-3.01888774004913E-48,-2.46519032881566E-32,
1.));
#23634=DIRECTION('center_axis',(-1.22460635382238E-16,-1.,-2.46519032881566E-32));
#23635=DIRECTION('ref_axis',(-3.01888774004913E-48,-2.46519032881566E-32,
1.));
#23636=DIRECTION('center_axis',(-1.22460635382238E-16,-1.,-2.46519032881566E-32));
#23637=DIRECTION('ref_axis',(-3.01888774004913E-48,-2.46519032881566E-32,
1.));
#23638=DIRECTION('center_axis',(-1.22460635382238E-16,-1.,-2.46519032881566E-32));
#23639=DIRECTION('ref_axis',(-3.01888774004913E-48,-2.46519032881566E-32,
1.));
#23640=DIRECTION('center_axis',(-1.22460635382238E-16,-1.,-2.46519032881566E-32));
#23641=DIRECTION('ref_axis',(-3.01888774004913E-48,-2.46519032881566E-32,
1.));
#23642=DIRECTION('center_axis',(-1.22460635382238E-16,-1.,-2.46519032881566E-32));
#23643=DIRECTION('ref_axis',(-3.01888774004913E-48,-2.46519032881566E-32,
1.));
#23644=DIRECTION('center_axis',(-1.22460635382238E-16,-1.,-2.46519032881566E-32));
#23645=DIRECTION('ref_axis',(-3.01888774004913E-48,-2.46519032881566E-32,
1.));
#23646=DIRECTION('center_axis',(-1.22460635382238E-16,-1.,-2.46519032881566E-32));
#23647=DIRECTION('ref_axis',(-3.01888774004913E-48,-2.46519032881566E-32,
1.));
#23648=DIRECTION('center_axis',(-1.22460635382238E-16,-1.,-2.46519032881566E-32));
#23649=DIRECTION('ref_axis',(-3.01888774004913E-48,-2.46519032881566E-32,
1.));
#23650=DIRECTION('center_axis',(-1.22460635382238E-16,-1.,-2.46519032881566E-32));
#23651=DIRECTION('ref_axis',(-3.01888774004913E-48,-2.46519032881566E-32,
1.));
#23652=DIRECTION('center_axis',(-1.22460635382238E-16,-1.,-2.46519032881566E-32));
#23653=DIRECTION('ref_axis',(-3.01888774004913E-48,-2.46519032881566E-32,
1.));
#23654=DIRECTION('center_axis',(-1.22460635382238E-16,-1.,-2.46519032881566E-32));
#23655=DIRECTION('ref_axis',(-3.01888774004913E-48,-2.46519032881566E-32,
1.));
#23656=DIRECTION('center_axis',(-1.22460635382238E-16,-1.,-2.46519032881566E-32));
#23657=DIRECTION('ref_axis',(-3.01888774004913E-48,-2.46519032881566E-32,
1.));
#23658=DIRECTION('center_axis',(-1.22460635382238E-16,-1.,-2.46519032881566E-32));
#23659=DIRECTION('ref_axis',(-3.01888774004913E-48,-2.46519032881566E-32,
1.));
#23660=DIRECTION('center_axis',(-1.22460635382238E-16,-1.,-2.46519032881566E-32));
#23661=DIRECTION('ref_axis',(-3.01888774004913E-48,-2.46519032881566E-32,
1.));
#23662=DIRECTION('center_axis',(-1.22460635382238E-16,-1.,-2.46519032881566E-32));
#23663=DIRECTION('ref_axis',(-3.01888774004913E-48,-2.46519032881566E-32,
1.));
#23664=DIRECTION('center_axis',(-1.22460635382238E-16,-1.,-2.46519032881566E-32));
#23665=DIRECTION('ref_axis',(-3.01888774004913E-48,-2.46519032881566E-32,
1.));
#23666=DIRECTION('center_axis',(-1.22460635382238E-16,-1.,-2.46519032881566E-32));
#23667=DIRECTION('ref_axis',(-3.01888774004913E-48,-2.46519032881566E-32,
1.));
#23668=DIRECTION('center_axis',(-1.22460635382238E-16,-1.,-2.46519032881566E-32));
#23669=DIRECTION('ref_axis',(-3.01888774004913E-48,-2.46519032881566E-32,
1.));
#23670=DIRECTION('center_axis',(-1.22460635382238E-16,-1.,-2.46519032881566E-32));
#23671=DIRECTION('ref_axis',(-3.01888774004913E-48,-2.46519032881566E-32,
1.));
#23672=DIRECTION('center_axis',(-1.22460635382238E-16,-1.,-2.46519032881566E-32));
#23673=DIRECTION('ref_axis',(-3.01888774004913E-48,-2.46519032881566E-32,
1.));
#23674=DIRECTION('center_axis',(-1.22460635382238E-16,-1.,-2.46519032881566E-32));
#23675=DIRECTION('ref_axis',(-3.01888774004913E-48,-2.46519032881566E-32,
1.));
#23676=DIRECTION('center_axis',(-1.22460635382238E-16,-1.,-2.46519032881566E-32));
#23677=DIRECTION('ref_axis',(-3.01888774004913E-48,-2.46519032881566E-32,
1.));
#23678=DIRECTION('center_axis',(-1.22460635382238E-16,-1.,-2.46519032881566E-32));
#23679=DIRECTION('ref_axis',(-3.01888774004913E-48,-2.46519032881566E-32,
1.));
#23680=DIRECTION('center_axis',(-1.22460635382238E-16,-1.,-2.46519032881566E-32));
#23681=DIRECTION('ref_axis',(-3.01888774004913E-48,-2.46519032881566E-32,
1.));
#23682=DIRECTION('center_axis',(-1.22460635382238E-16,-1.,-2.46519032881566E-32));
#23683=DIRECTION('ref_axis',(-3.01888774004913E-48,-2.46519032881566E-32,
1.));
#23684=DIRECTION('center_axis',(-1.22460635382238E-16,-1.,-2.46519032881566E-32));
#23685=DIRECTION('ref_axis',(-3.01888774004913E-48,-2.46519032881566E-32,
1.));
#23686=DIRECTION('center_axis',(-1.22460635382238E-16,-1.,-2.46519032881566E-32));
#23687=DIRECTION('ref_axis',(-3.01888774004913E-48,-2.46519032881566E-32,
1.));
#23688=DIRECTION('center_axis',(-1.22460635382238E-16,-1.,-2.46519032881566E-32));
#23689=DIRECTION('ref_axis',(-3.01888774004913E-48,-2.46519032881566E-32,
1.));
#23690=DIRECTION('center_axis',(-1.22460635382238E-16,-1.,-2.46519032881566E-32));
#23691=DIRECTION('ref_axis',(-3.01888774004913E-48,-2.46519032881566E-32,
1.));
#23692=DIRECTION('center_axis',(-1.22460635382238E-16,-1.,-2.46519032881566E-32));
#23693=DIRECTION('ref_axis',(-3.01888774004913E-48,-2.46519032881566E-32,
1.));
#23694=DIRECTION('center_axis',(-1.22460635382238E-16,-1.,-2.46519032881566E-32));
#23695=DIRECTION('ref_axis',(-3.01888774004913E-48,-2.46519032881566E-32,
1.));
#23696=DIRECTION('center_axis',(-1.22460635382238E-16,-1.,-2.46519032881566E-32));
#23697=DIRECTION('ref_axis',(-3.01888774004913E-48,-2.46519032881566E-32,
1.));
#23698=DIRECTION('center_axis',(-1.22460635382238E-16,-1.,-2.46519032881566E-32));
#23699=DIRECTION('ref_axis',(-3.01888774004913E-48,-2.46519032881566E-32,
1.));
#23700=DIRECTION('center_axis',(-1.22460635382238E-16,-1.,-2.46519032881566E-32));
#23701=DIRECTION('ref_axis',(-3.01888774004913E-48,-2.46519032881566E-32,
1.));
#23702=DIRECTION('center_axis',(-1.22460635382238E-16,-1.,-2.46519032881566E-32));
#23703=DIRECTION('ref_axis',(-3.01888774004913E-48,-2.46519032881566E-32,
1.));
#23704=DIRECTION('center_axis',(-1.22460635382238E-16,-1.,-2.46519032881566E-32));
#23705=DIRECTION('ref_axis',(-3.01888774004913E-48,-2.46519032881566E-32,
1.));
#23706=DIRECTION('center_axis',(1.22460635382238E-16,1.,2.46519032881566E-32));
#23707=DIRECTION('ref_axis',(3.01888774004913E-48,2.46519032881566E-32,
-1.));
#23708=DIRECTION('center_axis',(-1.22460635382238E-16,-1.,-2.46519032881566E-32));
#23709=DIRECTION('ref_axis',(-3.01888774004913E-48,-2.46519032881566E-32,
1.));
#23710=DIRECTION('center_axis',(-1.22460635382238E-16,-1.,-2.46519032881566E-32));
#23711=DIRECTION('ref_axis',(-3.01888774004913E-48,-2.46519032881566E-32,
1.));
#23712=DIRECTION('center_axis',(-1.22460635382238E-16,-1.,-2.46519032881566E-32));
#23713=DIRECTION('ref_axis',(-3.01888774004913E-48,-2.46519032881566E-32,
1.));
#23714=DIRECTION('center_axis',(-1.22460635382238E-16,-1.,-2.46519032881566E-32));
#23715=DIRECTION('ref_axis',(-3.01888774004913E-48,-2.46519032881566E-32,
1.));
#23716=DIRECTION('center_axis',(-1.22460635382238E-16,-1.,-2.46519032881566E-32));
#23717=DIRECTION('ref_axis',(-3.01888774004913E-48,-2.46519032881566E-32,
1.));
#23718=DIRECTION('center_axis',(-1.22460635382238E-16,-1.,-2.46519032881566E-32));
#23719=DIRECTION('ref_axis',(-3.01888774004913E-48,-2.46519032881566E-32,
1.));
#23720=DIRECTION('center_axis',(-1.22460635382238E-16,-1.,-2.46519032881566E-32));
#23721=DIRECTION('ref_axis',(-3.01888774004913E-48,-2.46519032881566E-32,
1.));
#23722=DIRECTION('center_axis',(-1.22460635382238E-16,-1.,-2.46519032881566E-32));
#23723=DIRECTION('ref_axis',(-3.01888774004913E-48,-2.46519032881566E-32,
1.));
#23724=DIRECTION('center_axis',(-1.22460635382238E-16,-1.,-2.46519032881566E-32));
#23725=DIRECTION('ref_axis',(-3.01888774004913E-48,-2.46519032881566E-32,
1.));
#23726=DIRECTION('center_axis',(-1.22460635382238E-16,-1.,-2.46519032881566E-32));
#23727=DIRECTION('ref_axis',(-3.01888774004913E-48,-2.46519032881566E-32,
1.));
#23728=DIRECTION('center_axis',(-1.22460635382238E-16,-1.,-2.46519032881566E-32));
#23729=DIRECTION('ref_axis',(-3.01888774004913E-48,-2.46519032881566E-32,
1.));
#23730=DIRECTION('center_axis',(-1.22460635382238E-16,-1.,-2.46519032881566E-32));
#23731=DIRECTION('ref_axis',(-3.01888774004913E-48,-2.46519032881566E-32,
1.));
#23732=DIRECTION('center_axis',(-1.22460635382238E-16,-1.,-2.46519032881566E-32));
#23733=DIRECTION('ref_axis',(-3.01888774004913E-48,-2.46519032881566E-32,
1.));
#23734=DIRECTION('center_axis',(-1.22460635382238E-16,-1.,-2.46519032881566E-32));
#23735=DIRECTION('ref_axis',(-3.01888774004913E-48,-2.46519032881566E-32,
1.));
#23736=DIRECTION('center_axis',(-1.22460635382238E-16,-1.,-2.46519032881566E-32));
#23737=DIRECTION('ref_axis',(-3.01888774004913E-48,-2.46519032881566E-32,
1.));
#23738=DIRECTION('center_axis',(-1.22460635382238E-16,-1.,-2.46519032881566E-32));
#23739=DIRECTION('ref_axis',(-3.01888774004913E-48,-2.46519032881566E-32,
1.));
#23740=DIRECTION('center_axis',(-1.22460635382238E-16,-1.,-2.46519032881566E-32));
#23741=DIRECTION('ref_axis',(-3.01888774004913E-48,-2.46519032881566E-32,
1.));
#23742=DIRECTION('center_axis',(-1.22460635382238E-16,-1.,-2.46519032881566E-32));
#23743=DIRECTION('ref_axis',(-3.01888774004913E-48,-2.46519032881566E-32,
1.));
#23744=DIRECTION('center_axis',(-1.22460635382238E-16,-1.,-2.46519032881566E-32));
#23745=DIRECTION('ref_axis',(-3.01888774004913E-48,-2.46519032881566E-32,
1.));
#23746=DIRECTION('center_axis',(-1.22460635382238E-16,-1.,-2.46519032881566E-32));
#23747=DIRECTION('ref_axis',(-3.01888774004913E-48,-2.46519032881566E-32,
1.));
#23748=DIRECTION('center_axis',(-1.22460635382238E-16,-1.,-2.46519032881566E-32));
#23749=DIRECTION('ref_axis',(-3.01888774004913E-48,-2.46519032881566E-32,
1.));
#23750=DIRECTION('center_axis',(-1.22460635382238E-16,-1.,-2.46519032881566E-32));
#23751=DIRECTION('ref_axis',(-3.01888774004913E-48,-2.46519032881566E-32,
1.));
#23752=DIRECTION('center_axis',(-1.22460635382238E-16,-1.,-2.46519032881566E-32));
#23753=DIRECTION('ref_axis',(-3.01888774004913E-48,-2.46519032881566E-32,
1.));
#23754=DIRECTION('center_axis',(-1.22460635382238E-16,-1.,-2.46519032881566E-32));
#23755=DIRECTION('ref_axis',(-3.01888774004913E-48,-2.46519032881566E-32,
1.));
#23756=DIRECTION('center_axis',(-1.22460635382238E-16,-1.,-2.46519032881566E-32));
#23757=DIRECTION('ref_axis',(-3.01888774004913E-48,-2.46519032881566E-32,
1.));
#23758=DIRECTION('center_axis',(-1.22460635382238E-16,-1.,-2.46519032881566E-32));
#23759=DIRECTION('ref_axis',(-3.01888774004913E-48,-2.46519032881566E-32,
1.));
#23760=DIRECTION('center_axis',(-1.22460635382238E-16,-1.,-2.46519032881566E-32));
#23761=DIRECTION('ref_axis',(-3.01888774004913E-48,-2.46519032881566E-32,
1.));
#23762=DIRECTION('center_axis',(-1.22460635382238E-16,-1.,-2.46519032881566E-32));
#23763=DIRECTION('ref_axis',(-3.01888774004913E-48,-2.46519032881566E-32,
1.));
#23764=DIRECTION('center_axis',(-1.22460635382238E-16,-1.,-2.46519032881566E-32));
#23765=DIRECTION('ref_axis',(-3.01888774004913E-48,-2.46519032881566E-32,
1.));
#23766=DIRECTION('center_axis',(-1.22460635382238E-16,-1.,-2.46519032881566E-32));
#23767=DIRECTION('ref_axis',(-3.01888774004913E-48,-2.46519032881566E-32,
1.));
#23768=DIRECTION('center_axis',(-1.22460635382238E-16,-1.,-2.46519032881566E-32));
#23769=DIRECTION('ref_axis',(-3.01888774004913E-48,-2.46519032881566E-32,
1.));
#23770=DIRECTION('center_axis',(-1.22460635382238E-16,-1.,-2.46519032881566E-32));
#23771=DIRECTION('ref_axis',(-3.01888774004913E-48,-2.46519032881566E-32,
1.));
#23772=DIRECTION('center_axis',(-1.22460635382238E-16,-1.,-2.46519032881566E-32));
#23773=DIRECTION('ref_axis',(-3.01888774004913E-48,-2.46519032881566E-32,
1.));
#23774=DIRECTION('center_axis',(-1.22460635382238E-16,-1.,-2.46519032881566E-32));
#23775=DIRECTION('ref_axis',(-3.01888774004913E-48,-2.46519032881566E-32,
1.));
#23776=DIRECTION('center_axis',(-1.22460635382238E-16,-1.,-2.46519032881566E-32));
#23777=DIRECTION('ref_axis',(-3.01888774004913E-48,-2.46519032881566E-32,
1.));
#23778=DIRECTION('center_axis',(-1.22460635382238E-16,-1.,-2.46519032881566E-32));
#23779=DIRECTION('ref_axis',(-3.01888774004913E-48,-2.46519032881566E-32,
1.));
#23780=DIRECTION('center_axis',(-1.22460635382238E-16,-1.,-2.46519032881566E-32));
#23781=DIRECTION('ref_axis',(-3.01888774004913E-48,-2.46519032881566E-32,
1.));
#23782=DIRECTION('center_axis',(-1.22460635382238E-16,-1.,-2.46519032881566E-32));
#23783=DIRECTION('ref_axis',(-3.01888774004913E-48,-2.46519032881566E-32,
1.));
#23784=DIRECTION('center_axis',(-1.22460635382238E-16,-1.,-2.46519032881566E-32));
#23785=DIRECTION('ref_axis',(-3.01888774004913E-48,-2.46519032881566E-32,
1.));
#23786=DIRECTION('',(-1.73188351330743E-16,-0.707106781186547,-0.707106781186548));
#23787=DIRECTION('center_axis',(-1.22460635382238E-16,-1.,-2.46519032881566E-32));
#23788=DIRECTION('ref_axis',(-3.01888774004913E-48,-2.46519032881566E-32,
1.));
#23789=DIRECTION('center_axis',(-1.22460635382238E-16,-1.,-2.46519032881566E-32));
#23790=DIRECTION('ref_axis',(-3.01888774004913E-48,-2.46519032881566E-32,
1.));
#23791=DIRECTION('center_axis',(-1.22460635382238E-16,-1.,-2.46519032881566E-32));
#23792=DIRECTION('ref_axis',(-3.01888774004913E-48,-2.46519032881566E-32,
1.));
#23793=DIRECTION('center_axis',(-1.22460635382238E-16,-1.,-2.46519032881566E-32));
#23794=DIRECTION('ref_axis',(-3.01888774004913E-48,-2.46519032881566E-32,
1.));
#23795=DIRECTION('center_axis',(-1.22460635382238E-16,-1.,-2.46519032881566E-32));
#23796=DIRECTION('ref_axis',(-3.01888774004913E-48,-2.46519032881566E-32,
1.));
#23797=DIRECTION('center_axis',(-1.22460635382238E-16,-1.,-2.46519032881566E-32));
#23798=DIRECTION('ref_axis',(-3.01888774004913E-48,-2.46519032881566E-32,
1.));
#23799=DIRECTION('center_axis',(-1.22460635382238E-16,-1.,-2.46519032881566E-32));
#23800=DIRECTION('ref_axis',(-3.01888774004913E-48,-2.46519032881566E-32,
1.));
#23801=DIRECTION('center_axis',(-1.22460635382238E-16,-1.,-2.46519032881566E-32));
#23802=DIRECTION('ref_axis',(-3.01888774004913E-48,-2.46519032881566E-32,
1.));
#23803=DIRECTION('center_axis',(-1.22460635382238E-16,-1.,-2.46519032881566E-32));
#23804=DIRECTION('ref_axis',(-3.01888774004913E-48,-2.46519032881566E-32,
1.));
#23805=DIRECTION('center_axis',(-1.22460635382238E-16,-1.,-2.46519032881566E-32));
#23806=DIRECTION('ref_axis',(-3.01888774004913E-48,-2.46519032881566E-32,
1.));
#23807=DIRECTION('center_axis',(-1.22460635382238E-16,-1.,-2.46519032881566E-32));
#23808=DIRECTION('ref_axis',(-3.01888774004913E-48,-2.46519032881566E-32,
1.));
#23809=DIRECTION('center_axis',(-1.22460635382238E-16,-1.,-2.46519032881566E-32));
#23810=DIRECTION('ref_axis',(-3.01888774004913E-48,-2.46519032881566E-32,
1.));
#23811=DIRECTION('center_axis',(-1.22460635382238E-16,-1.,-2.46519032881566E-32));
#23812=DIRECTION('ref_axis',(-3.01888774004913E-48,-2.46519032881566E-32,
1.));
#23813=DIRECTION('center_axis',(-1.22460635382238E-16,-1.,-2.46519032881566E-32));
#23814=DIRECTION('ref_axis',(-3.01888774004913E-48,-2.46519032881566E-32,
1.));
#23815=DIRECTION('center_axis',(-1.22460635382238E-16,-1.,-2.46519032881566E-32));
#23816=DIRECTION('ref_axis',(-3.01888774004913E-48,-2.46519032881566E-32,
1.));
#23817=DIRECTION('center_axis',(-1.22460635382238E-16,-1.,-2.46519032881566E-32));
#23818=DIRECTION('ref_axis',(-3.01888774004913E-48,-2.46519032881566E-32,
1.));
#23819=DIRECTION('center_axis',(-1.22460635382238E-16,-1.,-2.46519032881566E-32));
#23820=DIRECTION('ref_axis',(-3.01888774004913E-48,-2.46519032881566E-32,
1.));
#23821=DIRECTION('center_axis',(-1.22460635382238E-16,-1.,-2.46519032881566E-32));
#23822=DIRECTION('ref_axis',(-3.01888774004913E-48,-2.46519032881566E-32,
1.));
#23823=DIRECTION('center_axis',(-1.22460635382238E-16,-1.,-2.46519032881566E-32));
#23824=DIRECTION('ref_axis',(-3.01888774004913E-48,-2.46519032881566E-32,
1.));
#23825=DIRECTION('center_axis',(-1.22460635382238E-16,-1.,-2.46519032881566E-32));
#23826=DIRECTION('ref_axis',(-3.01888774004913E-48,-2.46519032881566E-32,
1.));
#23827=DIRECTION('center_axis',(-1.22460635382238E-16,-1.,-2.46519032881566E-32));
#23828=DIRECTION('ref_axis',(-3.01888774004913E-48,-2.46519032881566E-32,
1.));
#23829=DIRECTION('center_axis',(-1.22460635382238E-16,-1.,-2.46519032881566E-32));
#23830=DIRECTION('ref_axis',(-3.01888774004913E-48,-2.46519032881566E-32,
1.));
#23831=DIRECTION('center_axis',(-1.22460635382238E-16,-1.,-2.46519032881566E-32));
#23832=DIRECTION('ref_axis',(-3.01888774004913E-48,-2.46519032881566E-32,
1.));
#23833=DIRECTION('center_axis',(-1.22460635382238E-16,-1.,-2.46519032881566E-32));
#23834=DIRECTION('ref_axis',(-3.01888774004913E-48,-2.46519032881566E-32,
1.));
#23835=DIRECTION('center_axis',(-1.22460635382238E-16,-1.,-2.46519032881566E-32));
#23836=DIRECTION('ref_axis',(-3.01888774004913E-48,-2.46519032881566E-32,
1.));
#23837=DIRECTION('center_axis',(-1.22460635382238E-16,-1.,-2.46519032881566E-32));
#23838=DIRECTION('ref_axis',(-3.01888774004913E-48,-2.46519032881566E-32,
1.));
#23839=DIRECTION('center_axis',(-1.22460635382238E-16,-1.,-2.46519032881566E-32));
#23840=DIRECTION('ref_axis',(-3.01888774004913E-48,-2.46519032881566E-32,
1.));
#23841=DIRECTION('center_axis',(-1.22460635382238E-16,-1.,-2.46519032881566E-32));
#23842=DIRECTION('ref_axis',(-3.01888774004913E-48,-2.46519032881566E-32,
1.));
#23843=DIRECTION('center_axis',(-1.22460635382238E-16,-1.,-2.46519032881566E-32));
#23844=DIRECTION('ref_axis',(-3.01888774004913E-48,-2.46519032881566E-32,
1.));
#23845=DIRECTION('center_axis',(-1.22460635382238E-16,-1.,-2.46519032881566E-32));
#23846=DIRECTION('ref_axis',(-3.01888774004913E-48,-2.46519032881566E-32,
1.));
#23847=DIRECTION('center_axis',(-1.22460635382238E-16,-1.,-2.46519032881566E-32));
#23848=DIRECTION('ref_axis',(-3.01888774004913E-48,-2.46519032881566E-32,
1.));
#23849=DIRECTION('center_axis',(-1.22460635382238E-16,-1.,-2.46519032881566E-32));
#23850=DIRECTION('ref_axis',(-3.01888774004913E-48,-2.46519032881566E-32,
1.));
#23851=DIRECTION('center_axis',(-1.22460635382238E-16,-1.,-2.46519032881566E-32));
#23852=DIRECTION('ref_axis',(-3.01888774004913E-48,-2.46519032881566E-32,
1.));
#23853=DIRECTION('center_axis',(-1.22460635382238E-16,-1.,-2.46519032881566E-32));
#23854=DIRECTION('ref_axis',(-3.01888774004913E-48,-2.46519032881566E-32,
1.));
#23855=DIRECTION('center_axis',(-1.22460635382238E-16,-1.,-2.46519032881566E-32));
#23856=DIRECTION('ref_axis',(-3.01888774004913E-48,-2.46519032881566E-32,
1.));
#23857=DIRECTION('center_axis',(-1.22460635382238E-16,-1.,-2.46519032881566E-32));
#23858=DIRECTION('ref_axis',(-3.01888774004913E-48,-2.46519032881566E-32,
1.));
#23859=DIRECTION('center_axis',(-1.22460635382238E-16,-1.,-2.46519032881566E-32));
#23860=DIRECTION('ref_axis',(-3.01888774004913E-48,-2.46519032881566E-32,
1.));
#23861=DIRECTION('center_axis',(-1.22460635382238E-16,-1.,-2.46519032881566E-32));
#23862=DIRECTION('ref_axis',(-3.01888774004913E-48,-2.46519032881566E-32,
1.));
#23863=DIRECTION('center_axis',(-1.22460635382238E-16,-1.,-2.46519032881566E-32));
#23864=DIRECTION('ref_axis',(-3.01888774004913E-48,-2.46519032881566E-32,
1.));
#23865=DIRECTION('center_axis',(-1.22460635382238E-16,-1.,-2.46519032881566E-32));
#23866=DIRECTION('ref_axis',(-3.01888774004913E-48,-2.46519032881566E-32,
1.));
#23867=DIRECTION('center_axis',(-1.22460635382238E-16,-1.,-2.46519032881566E-32));
#23868=DIRECTION('ref_axis',(-3.01888774004913E-48,-2.46519032881566E-32,
1.));
#23869=DIRECTION('',(1.22460635382238E-16,1.,2.46519032881566E-32));
#23870=DIRECTION('center_axis',(-1.22460635382238E-16,-1.,-2.46519032881566E-32));
#23871=DIRECTION('ref_axis',(-3.01888774004913E-48,-2.46519032881566E-32,
1.));
#23872=DIRECTION('',(-1.22460635382238E-16,-1.,-2.46519032881566E-32));
#23873=DIRECTION('',(-1.22460635382238E-16,-1.,-2.46519032881566E-32));
#23874=DIRECTION('center_axis',(-1.22460635382238E-16,-1.,-2.46519032881566E-32));
#23875=DIRECTION('ref_axis',(-3.01888774004913E-48,-2.46519032881566E-32,
1.));
#23876=DIRECTION('',(-1.22460635382238E-16,-1.,-2.46519032881566E-32));
#23877=DIRECTION('',(-1.22460635382238E-16,-1.,-2.46519032881566E-32));
#23878=DIRECTION('center_axis',(-1.22460635382238E-16,-1.,-2.46519032881566E-32));
#23879=DIRECTION('ref_axis',(-3.01888774004913E-48,-2.46519032881566E-32,
1.));
#23880=DIRECTION('',(-1.22460635382238E-16,-1.,-2.46519032881566E-32));
#23881=DIRECTION('',(-1.22460635382238E-16,-1.,-2.46519032881566E-32));
#23882=DIRECTION('center_axis',(-1.22460635382238E-16,-1.,-2.46519032881566E-32));
#23883=DIRECTION('ref_axis',(-3.01888774004913E-48,-2.46519032881566E-32,
1.));
#23884=DIRECTION('',(-1.22460635382238E-16,-1.,-2.46519032881566E-32));
#23885=DIRECTION('',(-1.22460635382238E-16,-1.,-2.46519032881566E-32));
#23886=DIRECTION('center_axis',(-1.22460635382238E-16,-1.,-2.46519032881566E-32));
#23887=DIRECTION('ref_axis',(-3.01888774004913E-48,-2.46519032881566E-32,
1.));
#23888=DIRECTION('',(-1.22460635382238E-16,-1.,-2.46519032881566E-32));
#23889=DIRECTION('',(-1.22460635382238E-16,-1.,-2.46519032881566E-32));
#23890=DIRECTION('center_axis',(-1.22460635382238E-16,-1.,-2.46519032881566E-32));
#23891=DIRECTION('ref_axis',(-3.01888774004913E-48,-2.46519032881566E-32,
1.));
#23892=DIRECTION('',(-1.22460635382238E-16,-1.,-2.46519032881566E-32));
#23893=DIRECTION('',(-1.22460635382238E-16,-1.,-2.46519032881566E-32));
#23894=DIRECTION('center_axis',(-1.22460635382238E-16,-1.,-2.46519032881566E-32));
#23895=DIRECTION('ref_axis',(-3.01888774004913E-48,-2.46519032881566E-32,
1.));
#23896=DIRECTION('',(-1.22460635382238E-16,-1.,-2.46519032881566E-32));
#23897=DIRECTION('',(-1.22460635382238E-16,-1.,-2.46519032881566E-32));
#23898=DIRECTION('center_axis',(-1.22460635382238E-16,-1.,-2.46519032881566E-32));
#23899=DIRECTION('ref_axis',(-3.01888774004913E-48,-2.46519032881566E-32,
1.));
#23900=DIRECTION('',(-1.22460635382238E-16,-1.,-2.46519032881566E-32));
#23901=DIRECTION('',(-1.22460635382238E-16,-1.,-2.46519032881566E-32));
#23902=DIRECTION('center_axis',(-1.22460635382238E-16,-1.,-2.46519032881566E-32));
#23903=DIRECTION('ref_axis',(-3.01888774004913E-48,-2.46519032881566E-32,
1.));
#23904=DIRECTION('',(-1.22460635382238E-16,-1.,-2.46519032881566E-32));
#23905=DIRECTION('',(-1.22460635382238E-16,-1.,-2.46519032881566E-32));
#23906=DIRECTION('center_axis',(-1.22460635382238E-16,-1.,-2.46519032881566E-32));
#23907=DIRECTION('ref_axis',(-3.01888774004913E-48,-2.46519032881566E-32,
1.));
#23908=DIRECTION('',(-1.22460635382238E-16,-1.,-2.46519032881566E-32));
#23909=DIRECTION('',(-1.22460635382238E-16,-1.,-2.46519032881566E-32));
#23910=DIRECTION('center_axis',(-1.22460635382238E-16,-1.,-2.46519032881566E-32));
#23911=DIRECTION('ref_axis',(-3.01888774004913E-48,-2.46519032881566E-32,
1.));
#23912=DIRECTION('',(-1.22460635382238E-16,-1.,-2.46519032881566E-32));
#23913=DIRECTION('',(-1.22460635382238E-16,-1.,-2.46519032881566E-32));
#23914=DIRECTION('center_axis',(-1.22460635382238E-16,-1.,-2.46519032881566E-32));
#23915=DIRECTION('ref_axis',(-3.01888774004913E-48,-2.46519032881566E-32,
1.));
#23916=DIRECTION('',(-1.22460635382238E-16,-1.,-2.46519032881566E-32));
#23917=DIRECTION('',(-1.22460635382238E-16,-1.,-2.46519032881566E-32));
#23918=DIRECTION('center_axis',(-1.22460635382238E-16,-1.,-2.46519032881566E-32));
#23919=DIRECTION('ref_axis',(-3.01888774004913E-48,-2.46519032881566E-32,
1.));
#23920=DIRECTION('',(-1.22460635382238E-16,-1.,-2.46519032881566E-32));
#23921=DIRECTION('',(-1.22460635382238E-16,-1.,-2.46519032881566E-32));
#23922=DIRECTION('center_axis',(-1.22460635382238E-16,-1.,-2.46519032881566E-32));
#23923=DIRECTION('ref_axis',(-3.01888774004913E-48,-2.46519032881566E-32,
1.));
#23924=DIRECTION('',(-1.22460635382238E-16,-1.,-2.46519032881566E-32));
#23925=DIRECTION('',(-1.22460635382238E-16,-1.,-2.46519032881566E-32));
#23926=DIRECTION('center_axis',(-1.22460635382238E-16,-1.,-2.46519032881566E-32));
#23927=DIRECTION('ref_axis',(-3.01888774004913E-48,-2.46519032881566E-32,
1.));
#23928=DIRECTION('',(-1.22460635382238E-16,-1.,-2.46519032881566E-32));
#23929=DIRECTION('',(-1.22460635382238E-16,-1.,-2.46519032881566E-32));
#23930=DIRECTION('center_axis',(-1.22460635382238E-16,-1.,-2.46519032881566E-32));
#23931=DIRECTION('ref_axis',(-3.01888774004913E-48,-2.46519032881566E-32,
1.));
#23932=DIRECTION('',(-1.22460635382238E-16,-1.,-2.46519032881566E-32));
#23933=DIRECTION('',(-1.22460635382238E-16,-1.,-2.46519032881566E-32));
#23934=DIRECTION('center_axis',(-1.22460635382238E-16,-1.,-2.46519032881566E-32));
#23935=DIRECTION('ref_axis',(-3.01888774004913E-48,-2.46519032881566E-32,
1.));
#23936=DIRECTION('',(-1.22460635382238E-16,-1.,-2.46519032881566E-32));
#23937=DIRECTION('',(-1.22460635382238E-16,-1.,-2.46519032881566E-32));
#23938=DIRECTION('center_axis',(-1.22460635382238E-16,-1.,-2.46519032881566E-32));
#23939=DIRECTION('ref_axis',(-3.01888774004913E-48,-2.46519032881566E-32,
1.));
#23940=DIRECTION('',(-1.22460635382238E-16,-1.,-2.46519032881566E-32));
#23941=DIRECTION('',(-1.22460635382238E-16,-1.,-2.46519032881566E-32));
#23942=DIRECTION('center_axis',(-1.22460635382238E-16,-1.,-2.46519032881566E-32));
#23943=DIRECTION('ref_axis',(-3.01888774004913E-48,-2.46519032881566E-32,
1.));
#23944=DIRECTION('',(-1.22460635382238E-16,-1.,-2.46519032881566E-32));
#23945=DIRECTION('',(-1.22460635382238E-16,-1.,-2.46519032881566E-32));
#23946=DIRECTION('center_axis',(-1.22460635382238E-16,-1.,-2.46519032881566E-32));
#23947=DIRECTION('ref_axis',(-3.01888774004913E-48,-2.46519032881566E-32,
1.));
#23948=DIRECTION('',(-1.22460635382238E-16,-1.,-2.46519032881566E-32));
#23949=DIRECTION('',(-1.22460635382238E-16,-1.,-2.46519032881566E-32));
#23950=DIRECTION('center_axis',(-1.22460635382238E-16,-1.,-2.46519032881566E-32));
#23951=DIRECTION('ref_axis',(-3.01888774004913E-48,-2.46519032881566E-32,
1.));
#23952=DIRECTION('',(-1.22460635382238E-16,-1.,-2.46519032881566E-32));
#23953=DIRECTION('',(-1.22460635382238E-16,-1.,-2.46519032881566E-32));
#23954=DIRECTION('center_axis',(-1.22460635382238E-16,-1.,-2.46519032881566E-32));
#23955=DIRECTION('ref_axis',(-3.01888774004913E-48,-2.46519032881566E-32,
1.));
#23956=DIRECTION('',(-1.22460635382238E-16,-1.,-2.46519032881566E-32));
#23957=DIRECTION('',(-1.22460635382238E-16,-1.,-2.46519032881566E-32));
#23958=DIRECTION('center_axis',(-1.22460635382238E-16,-1.,-2.46519032881566E-32));
#23959=DIRECTION('ref_axis',(-3.01888774004913E-48,-2.46519032881566E-32,
1.));
#23960=DIRECTION('',(-1.22460635382238E-16,-1.,-2.46519032881566E-32));
#23961=DIRECTION('',(-1.22460635382238E-16,-1.,-2.46519032881566E-32));
#23962=DIRECTION('center_axis',(-1.22460635382238E-16,-1.,-2.46519032881566E-32));
#23963=DIRECTION('ref_axis',(-3.01888774004913E-48,-2.46519032881566E-32,
1.));
#23964=DIRECTION('',(-1.22460635382238E-16,-1.,-2.46519032881566E-32));
#23965=DIRECTION('',(-1.22460635382238E-16,-1.,-2.46519032881566E-32));
#23966=DIRECTION('center_axis',(-1.22460635382238E-16,-1.,-2.46519032881566E-32));
#23967=DIRECTION('ref_axis',(-3.01888774004913E-48,-2.46519032881566E-32,
1.));
#23968=DIRECTION('',(-1.22460635382238E-16,-1.,-2.46519032881566E-32));
#23969=DIRECTION('',(-1.22460635382238E-16,-1.,-2.46519032881566E-32));
#23970=DIRECTION('center_axis',(-1.22460635382238E-16,-1.,-2.46519032881566E-32));
#23971=DIRECTION('ref_axis',(-3.01888774004913E-48,-2.46519032881566E-32,
1.));
#23972=DIRECTION('',(-1.22460635382238E-16,-1.,-2.46519032881566E-32));
#23973=DIRECTION('',(-1.22460635382238E-16,-1.,-2.46519032881566E-32));
#23974=DIRECTION('center_axis',(-1.22460635382238E-16,-1.,-2.46519032881566E-32));
#23975=DIRECTION('ref_axis',(-3.01888774004913E-48,-2.46519032881566E-32,
1.));
#23976=DIRECTION('',(-1.22460635382238E-16,-1.,-2.46519032881566E-32));
#23977=DIRECTION('',(-1.22460635382238E-16,-1.,-2.46519032881566E-32));
#23978=DIRECTION('center_axis',(-1.22460635382238E-16,-1.,-2.46519032881566E-32));
#23979=DIRECTION('ref_axis',(-3.01888774004913E-48,-2.46519032881566E-32,
1.));
#23980=DIRECTION('',(-1.22460635382238E-16,-1.,-2.46519032881566E-32));
#23981=DIRECTION('',(-1.22460635382238E-16,-1.,-2.46519032881566E-32));
#23982=DIRECTION('center_axis',(-1.22460635382238E-16,-1.,-2.46519032881566E-32));
#23983=DIRECTION('ref_axis',(-3.01888774004913E-48,-2.46519032881566E-32,
1.));
#23984=DIRECTION('',(-1.22460635382238E-16,-1.,-2.46519032881566E-32));
#23985=DIRECTION('',(-1.22460635382238E-16,-1.,-2.46519032881566E-32));
#23986=DIRECTION('center_axis',(-1.22460635382238E-16,-1.,-2.46519032881566E-32));
#23987=DIRECTION('ref_axis',(-3.01888774004913E-48,-2.46519032881566E-32,
1.));
#23988=DIRECTION('',(-1.22460635382238E-16,-1.,-2.46519032881566E-32));
#23989=DIRECTION('',(-1.22460635382238E-16,-1.,-2.46519032881566E-32));
#23990=DIRECTION('center_axis',(-1.22460635382238E-16,-1.,-2.46519032881566E-32));
#23991=DIRECTION('ref_axis',(-3.01888774004913E-48,-2.46519032881566E-32,
1.));
#23992=DIRECTION('',(-1.22460635382238E-16,-1.,-2.46519032881566E-32));
#23993=DIRECTION('',(-1.22460635382238E-16,-1.,-2.46519032881566E-32));
#23994=DIRECTION('center_axis',(-1.22460635382238E-16,-1.,-2.46519032881566E-32));
#23995=DIRECTION('ref_axis',(-3.01888774004913E-48,-2.46519032881566E-32,
1.));
#23996=DIRECTION('',(-1.22460635382238E-16,-1.,-2.46519032881566E-32));
#23997=DIRECTION('',(-1.22460635382238E-16,-1.,-2.46519032881566E-32));
#23998=DIRECTION('center_axis',(-1.22460635382238E-16,-1.,-2.46519032881566E-32));
#23999=DIRECTION('ref_axis',(-3.01888774004913E-48,-2.46519032881566E-32,
1.));
#24000=DIRECTION('',(-1.22460635382238E-16,-1.,-2.46519032881566E-32));
#24001=DIRECTION('',(-1.22460635382238E-16,-1.,-2.46519032881566E-32));
#24002=DIRECTION('center_axis',(-1.22460635382238E-16,-1.,-2.46519032881566E-32));
#24003=DIRECTION('ref_axis',(-3.01888774004913E-48,-2.46519032881566E-32,
1.));
#24004=DIRECTION('',(-1.22460635382238E-16,-1.,-2.46519032881566E-32));
#24005=DIRECTION('',(-1.22460635382238E-16,-1.,-2.46519032881566E-32));
#24006=DIRECTION('center_axis',(-1.22460635382238E-16,-1.,-2.46519032881566E-32));
#24007=DIRECTION('ref_axis',(-3.01888774004913E-48,-2.46519032881566E-32,
1.));
#24008=DIRECTION('',(-1.22460635382238E-16,-1.,-2.46519032881566E-32));
#24009=DIRECTION('',(-1.22460635382238E-16,-1.,-2.46519032881566E-32));
#24010=DIRECTION('center_axis',(-1.22460635382238E-16,-1.,-2.46519032881566E-32));
#24011=DIRECTION('ref_axis',(-3.01888774004913E-48,-2.46519032881566E-32,
1.));
#24012=DIRECTION('',(-1.22460635382238E-16,-1.,-2.46519032881566E-32));
#24013=DIRECTION('',(-1.22460635382238E-16,-1.,-2.46519032881566E-32));
#24014=DIRECTION('center_axis',(-1.22460635382238E-16,-1.,-2.46519032881566E-32));
#24015=DIRECTION('ref_axis',(-3.01888774004913E-48,-2.46519032881566E-32,
1.));
#24016=DIRECTION('',(-1.22460635382238E-16,-1.,-2.46519032881566E-32));
#24017=DIRECTION('',(-1.22460635382238E-16,-1.,-2.46519032881566E-32));
#24018=DIRECTION('center_axis',(-1.22460635382238E-16,-1.,-2.46519032881566E-32));
#24019=DIRECTION('ref_axis',(-3.01888774004913E-48,-2.46519032881566E-32,
1.));
#24020=DIRECTION('',(-1.22460635382238E-16,-1.,-2.46519032881566E-32));
#24021=DIRECTION('',(-1.22460635382238E-16,-1.,-2.46519032881566E-32));
#24022=DIRECTION('center_axis',(-1.22460635382238E-16,-1.,-2.46519032881566E-32));
#24023=DIRECTION('ref_axis',(-3.01888774004913E-48,-2.46519032881566E-32,
1.));
#24024=DIRECTION('',(-1.22460635382238E-16,-1.,-2.46519032881566E-32));
#24025=DIRECTION('',(-1.22460635382238E-16,-1.,-2.46519032881566E-32));
#24026=DIRECTION('center_axis',(-1.22460635382238E-16,-1.,-2.46519032881566E-32));
#24027=DIRECTION('ref_axis',(-3.01888774004913E-48,-2.46519032881566E-32,
1.));
#24028=DIRECTION('',(-1.22460635382238E-16,-1.,-2.46519032881566E-32));
#24029=DIRECTION('',(-1.22460635382238E-16,-1.,-2.46519032881566E-32));
#24030=DIRECTION('center_axis',(-1.22460635382238E-16,-1.,-2.46519032881566E-32));
#24031=DIRECTION('ref_axis',(-3.01888774004913E-48,-2.46519032881566E-32,
1.));
#24032=DIRECTION('',(-1.22460635382238E-16,-1.,-2.46519032881566E-32));
#24033=DIRECTION('',(-1.22460635382238E-16,-1.,-2.46519032881566E-32));
#24034=DIRECTION('center_axis',(-1.22460635382238E-16,-1.,-2.46519032881566E-32));
#24035=DIRECTION('ref_axis',(-3.01888774004913E-48,-2.46519032881566E-32,
1.));
#24036=DIRECTION('',(-1.22460635382238E-16,-1.,-2.46519032881566E-32));
#24037=DIRECTION('',(-1.22460635382238E-16,-1.,-2.46519032881566E-32));
#24038=DIRECTION('center_axis',(-1.22460635382238E-16,-1.,-2.46519032881566E-32));
#24039=DIRECTION('ref_axis',(-3.01888774004913E-48,-2.46519032881566E-32,
1.));
#24040=DIRECTION('',(-1.22460635382238E-16,-1.,-2.46519032881566E-32));
#24041=DIRECTION('',(-1.22460635382238E-16,-1.,-2.46519032881566E-32));
#24042=DIRECTION('center_axis',(-1.22460635382238E-16,-1.,-2.46519032881566E-32));
#24043=DIRECTION('ref_axis',(-3.01888774004913E-48,-2.46519032881566E-32,
1.));
#24044=DIRECTION('',(-1.22460635382238E-16,-1.,-2.46519032881566E-32));
#24045=DIRECTION('',(-1.22460635382238E-16,-1.,-2.46519032881566E-32));
#24046=DIRECTION('center_axis',(-1.22460635382238E-16,-1.,-2.46519032881566E-32));
#24047=DIRECTION('ref_axis',(-3.01888774004913E-48,-2.46519032881566E-32,
1.));
#24048=DIRECTION('',(-1.22460635382238E-16,-1.,-2.46519032881566E-32));
#24049=DIRECTION('',(-1.22460635382238E-16,-1.,-2.46519032881566E-32));
#24050=DIRECTION('center_axis',(-1.22460635382238E-16,-1.,-2.46519032881566E-32));
#24051=DIRECTION('ref_axis',(-3.01888774004913E-48,-2.46519032881566E-32,
1.));
#24052=DIRECTION('',(-1.22460635382238E-16,-1.,-2.46519032881566E-32));
#24053=DIRECTION('',(-1.22460635382238E-16,-1.,-2.46519032881566E-32));
#24054=DIRECTION('center_axis',(-1.22460635382238E-16,-1.,-2.46519032881566E-32));
#24055=DIRECTION('ref_axis',(-3.01888774004913E-48,-2.46519032881566E-32,
1.));
#24056=DIRECTION('',(-1.22460635382238E-16,-1.,-2.46519032881566E-32));
#24057=DIRECTION('',(-1.22460635382238E-16,-1.,-2.46519032881566E-32));
#24058=DIRECTION('center_axis',(-1.22460635382238E-16,-1.,-2.46519032881566E-32));
#24059=DIRECTION('ref_axis',(-3.01888774004913E-48,-2.46519032881566E-32,
1.));
#24060=DIRECTION('',(-1.22460635382238E-16,-1.,-2.46519032881566E-32));
#24061=DIRECTION('',(-1.22460635382238E-16,-1.,-2.46519032881566E-32));
#24062=DIRECTION('center_axis',(-1.22460635382238E-16,-1.,-2.46519032881566E-32));
#24063=DIRECTION('ref_axis',(-3.01888774004913E-48,-2.46519032881566E-32,
1.));
#24064=DIRECTION('',(-1.22460635382238E-16,-1.,-2.46519032881566E-32));
#24065=DIRECTION('',(-1.22460635382238E-16,-1.,-2.46519032881566E-32));
#24066=DIRECTION('center_axis',(-1.22460635382238E-16,-1.,-2.46519032881566E-32));
#24067=DIRECTION('ref_axis',(-3.01888774004913E-48,-2.46519032881566E-32,
1.));
#24068=DIRECTION('',(-1.22460635382238E-16,-1.,-2.46519032881566E-32));
#24069=DIRECTION('',(-1.22460635382238E-16,-1.,-2.46519032881566E-32));
#24070=DIRECTION('center_axis',(-1.22460635382238E-16,-1.,-2.46519032881566E-32));
#24071=DIRECTION('ref_axis',(-3.01888774004913E-48,-2.46519032881566E-32,
1.));
#24072=DIRECTION('',(-1.22460635382238E-16,-1.,-2.46519032881566E-32));
#24073=DIRECTION('',(-1.22460635382238E-16,-1.,-2.46519032881566E-32));
#24074=DIRECTION('center_axis',(-1.22460635382238E-16,-1.,-2.46519032881566E-32));
#24075=DIRECTION('ref_axis',(-3.01888774004913E-48,-2.46519032881566E-32,
1.));
#24076=DIRECTION('',(-1.22460635382238E-16,-1.,-2.46519032881566E-32));
#24077=DIRECTION('',(-1.22460635382238E-16,-1.,-2.46519032881566E-32));
#24078=DIRECTION('center_axis',(-1.22460635382238E-16,-1.,-2.46519032881566E-32));
#24079=DIRECTION('ref_axis',(-3.01888774004913E-48,-2.46519032881566E-32,
1.));
#24080=DIRECTION('',(-1.22460635382238E-16,-1.,-2.46519032881566E-32));
#24081=DIRECTION('',(-1.22460635382238E-16,-1.,-2.46519032881566E-32));
#24082=DIRECTION('center_axis',(-1.22460635382238E-16,-1.,-2.46519032881566E-32));
#24083=DIRECTION('ref_axis',(-3.01888774004913E-48,-2.46519032881566E-32,
1.));
#24084=DIRECTION('',(-1.22460635382238E-16,-1.,-2.46519032881566E-32));
#24085=DIRECTION('',(-1.22460635382238E-16,-1.,-2.46519032881566E-32));
#24086=DIRECTION('center_axis',(-1.22460635382238E-16,-1.,-2.46519032881566E-32));
#24087=DIRECTION('ref_axis',(-3.01888774004913E-48,-2.46519032881566E-32,
1.));
#24088=DIRECTION('',(-1.22460635382238E-16,-1.,-2.46519032881566E-32));
#24089=DIRECTION('',(-1.22460635382238E-16,-1.,-2.46519032881566E-32));
#24090=DIRECTION('center_axis',(-1.22460635382238E-16,-1.,-2.46519032881566E-32));
#24091=DIRECTION('ref_axis',(-3.01888774004913E-48,-2.46519032881566E-32,
1.));
#24092=DIRECTION('',(-1.22460635382238E-16,-1.,-2.46519032881566E-32));
#24093=DIRECTION('',(-1.22460635382238E-16,-1.,-2.46519032881566E-32));
#24094=DIRECTION('center_axis',(-1.22460635382238E-16,-1.,-2.46519032881566E-32));
#24095=DIRECTION('ref_axis',(-3.01888774004913E-48,-2.46519032881566E-32,
1.));
#24096=DIRECTION('',(-1.22460635382238E-16,-1.,-2.46519032881566E-32));
#24097=DIRECTION('',(-1.22460635382238E-16,-1.,-2.46519032881566E-32));
#24098=DIRECTION('center_axis',(-1.22460635382238E-16,-1.,-2.46519032881566E-32));
#24099=DIRECTION('ref_axis',(-3.01888774004913E-48,-2.46519032881566E-32,
1.));
#24100=DIRECTION('',(-1.22460635382238E-16,-1.,-2.46519032881566E-32));
#24101=DIRECTION('',(-1.22460635382238E-16,-1.,-2.46519032881566E-32));
#24102=DIRECTION('center_axis',(-1.22460635382238E-16,-1.,-2.46519032881566E-32));
#24103=DIRECTION('ref_axis',(-3.01888774004913E-48,-2.46519032881566E-32,
1.));
#24104=DIRECTION('',(-1.22460635382238E-16,-1.,-2.46519032881566E-32));
#24105=DIRECTION('',(-1.22460635382238E-16,-1.,-2.46519032881566E-32));
#24106=DIRECTION('center_axis',(-1.22460635382238E-16,-1.,-2.46519032881566E-32));
#24107=DIRECTION('ref_axis',(-3.01888774004913E-48,-2.46519032881566E-32,
1.));
#24108=DIRECTION('',(-1.22460635382238E-16,-1.,-2.46519032881566E-32));
#24109=DIRECTION('',(-1.22460635382238E-16,-1.,-2.46519032881566E-32));
#24110=DIRECTION('center_axis',(-1.22460635382238E-16,-1.,-2.46519032881566E-32));
#24111=DIRECTION('ref_axis',(-3.01888774004913E-48,-2.46519032881566E-32,
1.));
#24112=DIRECTION('',(-1.22460635382238E-16,-1.,-2.46519032881566E-32));
#24113=DIRECTION('',(-1.22460635382238E-16,-1.,-2.46519032881566E-32));
#24114=DIRECTION('center_axis',(-1.22460635382238E-16,-1.,-2.46519032881566E-32));
#24115=DIRECTION('ref_axis',(-3.01888774004913E-48,-2.46519032881566E-32,
1.));
#24116=DIRECTION('',(-1.22460635382238E-16,-1.,-2.46519032881566E-32));
#24117=DIRECTION('',(-1.22460635382238E-16,-1.,-2.46519032881566E-32));
#24118=DIRECTION('center_axis',(-1.22460635382238E-16,-1.,-2.46519032881566E-32));
#24119=DIRECTION('ref_axis',(-3.01888774004913E-48,-2.46519032881566E-32,
1.));
#24120=DIRECTION('',(-1.22460635382238E-16,-1.,-2.46519032881566E-32));
#24121=DIRECTION('',(-1.22460635382238E-16,-1.,-2.46519032881566E-32));
#24122=DIRECTION('center_axis',(-1.22460635382238E-16,-1.,-2.46519032881566E-32));
#24123=DIRECTION('ref_axis',(-3.01888774004913E-48,-2.46519032881566E-32,
1.));
#24124=DIRECTION('',(-1.22460635382238E-16,-1.,-2.46519032881566E-32));
#24125=DIRECTION('',(-1.22460635382238E-16,-1.,-2.46519032881566E-32));
#24126=DIRECTION('center_axis',(-1.22460635382238E-16,-1.,-2.46519032881566E-32));
#24127=DIRECTION('ref_axis',(-3.01888774004913E-48,-2.46519032881566E-32,
1.));
#24128=DIRECTION('',(-1.22460635382238E-16,-1.,-2.46519032881566E-32));
#24129=DIRECTION('',(-1.22460635382238E-16,-1.,-2.46519032881566E-32));
#24130=DIRECTION('center_axis',(-1.22460635382238E-16,-1.,-2.46519032881566E-32));
#24131=DIRECTION('ref_axis',(-3.01888774004913E-48,-2.46519032881566E-32,
1.));
#24132=DIRECTION('',(-1.22460635382238E-16,-1.,-2.46519032881566E-32));
#24133=DIRECTION('',(-1.22460635382238E-16,-1.,-2.46519032881566E-32));
#24134=DIRECTION('center_axis',(-1.22460635382238E-16,-1.,-2.46519032881566E-32));
#24135=DIRECTION('ref_axis',(-3.01888774004913E-48,-2.46519032881566E-32,
1.));
#24136=DIRECTION('',(-1.22460635382238E-16,-1.,-2.46519032881566E-32));
#24137=DIRECTION('',(-1.22460635382238E-16,-1.,-2.46519032881566E-32));
#24138=DIRECTION('center_axis',(-1.22460635382238E-16,-1.,-2.46519032881566E-32));
#24139=DIRECTION('ref_axis',(-3.01888774004913E-48,-2.46519032881566E-32,
1.));
#24140=DIRECTION('',(-1.22460635382238E-16,-1.,-2.46519032881566E-32));
#24141=DIRECTION('',(-1.22460635382238E-16,-1.,-2.46519032881566E-32));
#24142=DIRECTION('center_axis',(-1.22460635382238E-16,-1.,-2.46519032881566E-32));
#24143=DIRECTION('ref_axis',(-3.01888774004913E-48,-2.46519032881566E-32,
1.));
#24144=DIRECTION('',(-1.22460635382238E-16,-1.,-2.46519032881566E-32));
#24145=DIRECTION('',(-1.22460635382238E-16,-1.,-2.46519032881566E-32));
#24146=DIRECTION('center_axis',(-1.22460635382238E-16,-1.,-2.46519032881566E-32));
#24147=DIRECTION('ref_axis',(-3.01888774004913E-48,-2.46519032881566E-32,
1.));
#24148=DIRECTION('',(-1.22460635382238E-16,-1.,-2.46519032881566E-32));
#24149=DIRECTION('',(-1.22460635382238E-16,-1.,-2.46519032881566E-32));
#24150=DIRECTION('center_axis',(-1.22460635382238E-16,-1.,-2.46519032881566E-32));
#24151=DIRECTION('ref_axis',(-3.01888774004913E-48,-2.46519032881566E-32,
1.));
#24152=DIRECTION('',(-1.22460635382238E-16,-1.,-2.46519032881566E-32));
#24153=DIRECTION('',(-1.22460635382238E-16,-1.,-2.46519032881566E-32));
#24154=DIRECTION('center_axis',(-1.22460635382238E-16,-1.,-2.46519032881566E-32));
#24155=DIRECTION('ref_axis',(-3.01888774004913E-48,-2.46519032881566E-32,
1.));
#24156=DIRECTION('',(-1.22460635382238E-16,-1.,-2.46519032881566E-32));
#24157=DIRECTION('',(-1.22460635382238E-16,-1.,-2.46519032881566E-32));
#24158=DIRECTION('center_axis',(-1.22460635382238E-16,-1.,-2.46519032881566E-32));
#24159=DIRECTION('ref_axis',(-3.01888774004913E-48,-2.46519032881566E-32,
1.));
#24160=DIRECTION('',(-1.22460635382238E-16,-1.,-2.46519032881566E-32));
#24161=DIRECTION('',(-1.22460635382238E-16,-1.,-2.46519032881566E-32));
#24162=DIRECTION('center_axis',(-1.22460635382238E-16,-1.,-2.46519032881566E-32));
#24163=DIRECTION('ref_axis',(-3.01888774004913E-48,-2.46519032881566E-32,
1.));
#24164=DIRECTION('',(-1.22460635382238E-16,-1.,-2.46519032881566E-32));
#24165=DIRECTION('',(-1.22460635382238E-16,-1.,-2.46519032881566E-32));
#24166=DIRECTION('center_axis',(-1.22460635382238E-16,-1.,-2.46519032881566E-32));
#24167=DIRECTION('ref_axis',(-3.01888774004913E-48,-2.46519032881566E-32,
1.));
#24168=DIRECTION('',(-1.22460635382238E-16,-1.,-2.46519032881566E-32));
#24169=DIRECTION('',(-1.22460635382238E-16,-1.,-2.46519032881566E-32));
#24170=DIRECTION('center_axis',(-1.22460635382238E-16,-1.,-2.46519032881566E-32));
#24171=DIRECTION('ref_axis',(-3.01888774004913E-48,-2.46519032881566E-32,
1.));
#24172=DIRECTION('',(-1.22460635382238E-16,-1.,-2.46519032881566E-32));
#24173=DIRECTION('',(-1.22460635382238E-16,-1.,-2.46519032881566E-32));
#24174=DIRECTION('center_axis',(-1.22460635382238E-16,-1.,-2.46519032881566E-32));
#24175=DIRECTION('ref_axis',(2.46519032881566E-32,-2.46519032881566E-32,
1.));
#24176=DIRECTION('center_axis',(-1.22460635382238E-16,-1.,-2.46519032881566E-32));
#24177=DIRECTION('ref_axis',(-3.01888774004913E-48,-2.46519032881566E-32,
1.));
#24178=DIRECTION('',(-1.22460635382238E-16,-1.,-2.46519032881566E-32));
#24179=DIRECTION('',(-1.22460635382238E-16,-1.,-2.46519032881566E-32));
#24180=DIRECTION('center_axis',(-1.22460635382238E-16,-1.,-2.46519032881566E-32));
#24181=DIRECTION('ref_axis',(2.46519032881566E-32,-2.46519032881566E-32,
1.));
#24182=DIRECTION('center_axis',(1.22460635382238E-16,1.,2.46519032881566E-32));
#24183=DIRECTION('ref_axis',(-2.46519032881566E-32,2.46519032881566E-32,
-1.));
#24184=DIRECTION('center_axis',(1.22460635382238E-16,1.,2.46519032881566E-32));
#24185=DIRECTION('ref_axis',(-2.46519032881566E-32,2.46519032881566E-32,
-1.));
#24186=DIRECTION('center_axis',(0.499999999999999,-6.12303176911187E-17,
-0.866025403784439));
#24187=DIRECTION('ref_axis',(-0.866025403784439,1.06054021204601E-16,-0.499999999999999));
#24188=DIRECTION('',(-1.22460635382238E-16,-1.,-2.46519032881566E-32));
#24189=DIRECTION('center_axis',(0.500000000000002,-6.12303176911191E-17,
0.866025403784438));
#24190=DIRECTION('ref_axis',(0.866025403784438,-1.06054021204601E-16,-0.500000000000002));
#24191=DIRECTION('center_axis',(0.427747181051069,-5.2382191574475E-17,
-0.903898417468945));
#24192=DIRECTION('ref_axis',(-0.903898417468945,1.10691974524246E-16,-0.427747181051069));
#24193=DIRECTION('',(-1.22460635382238E-16,-1.,-2.46519032881566E-32));
#24194=DIRECTION('center_axis',(0.568925401443124,-6.96709661458196E-17,
0.82238913392188));
#24195=DIRECTION('ref_axis',(0.82238913392188,-1.00710295871522E-16,-0.568925401443124));
#24196=DIRECTION('center_axis',(0.568925401443111,-6.9670966145818E-17,
-0.82238913392189));
#24197=DIRECTION('ref_axis',(-0.82238913392189,1.00710295871523E-16,-0.568925401443111));
#24198=DIRECTION('',(-1.22460635382238E-16,-1.,-2.46519032881566E-32));
#24199=DIRECTION('center_axis',(0.427747181051084,-5.23821915744769E-17,
0.903898417468938));
#24200=DIRECTION('ref_axis',(0.903898417468938,-1.10691974524245E-16,-0.427747181051084));
#24201=DIRECTION('center_axis',(0.634064698205714,-7.76479658157185E-17,
-0.773280000057739));
#24202=DIRECTION('ref_axis',(-0.773280000057739,9.46963601354476E-17,-0.634064698205714));
#24203=DIRECTION('',(-1.22460635382238E-16,-1.,-2.46519032881566E-32));
#24204=DIRECTION('center_axis',(0.352647775185578,-4.31854706153584E-17,
0.935756136317931));
#24205=DIRECTION('ref_axis',(0.935756136317931,-1.14593291016322E-16,-0.352647775185578));
#24206=DIRECTION('center_axis',(0.694984399015069,-8.5108231084128E-17,
-0.719024815375425));
#24207=DIRECTION('ref_axis',(-0.719024815375425,8.80522357464707E-17,-0.694984399015069));
#24208=DIRECTION('',(-1.22460635382238E-16,-1.,-2.46519032881566E-32));
#24209=DIRECTION('center_axis',(0.275201556558999,-3.37013574743959E-17,
0.961386552468623));
#24210=DIRECTION('ref_axis',(0.961386552468623,-1.17732008063247E-16,-0.275201556558999));
#24211=DIRECTION('center_axis',(0.751279093313334,-9.20021151165424E-17,
-0.65998463917753));
#24212=DIRECTION('ref_axis',(-0.65998463917753,8.08221382561973E-17,-0.751279093313334));
#24213=DIRECTION('',(-1.22460635382238E-16,-1.,-2.46519032881566E-32));
#24214=DIRECTION('center_axis',(0.195923916978581,-2.39929673597738E-17,
0.980619099730252));
#24215=DIRECTION('ref_axis',(0.980619099730252,-1.20087238020925E-16,-0.195923916978581));
#24216=DIRECTION('center_axis',(0.802574149197924,-9.82837402521366E-17,
-0.59655237409571));
#24217=DIRECTION('ref_axis',(-0.59655237409571,7.3054182770543E-17,-0.802574149197924));
#24218=DIRECTION('',(-1.22460635382238E-16,-1.,-2.46519032881566E-32));
#24219=DIRECTION('center_axis',(0.115342436055841,-1.41249080059334E-17,
0.99332578867394));
#24220=DIRECTION('ref_axis',(0.99332578867394,-1.21643307222573E-16,-0.115342436055841));
#24221=DIRECTION('center_axis',(0.848528206535016,-1.03911303312029E-16,
-0.529150151388497));
#24222=DIRECTION('ref_axis',(-0.529150151388497,6.48000637516426E-17,-0.848528206535016));
#24223=DIRECTION('',(-1.22460635382238E-16,-1.,-2.46519032881566E-32));
#24224=DIRECTION('center_axis',(0.033993370251312,-4.16284971975936E-18,
0.999422058381221));
#24225=DIRECTION('ref_axis',(0.999422058381221,-1.22389860284388E-16,-0.033993370251312));
#24226=DIRECTION('center_axis',(0.888835448654917,-1.08847353792537E-16,
-0.458226521727423));
#24227=DIRECTION('ref_axis',(-0.458226521727423,5.6114710999733E-17,-0.888835448654917));
#24228=DIRECTION('',(-1.22460635382238E-16,-1.,-2.46519032881566E-32));
#24229=DIRECTION('center_axis',(-0.047581915823728,5.82691164447786E-18,
0.998867339183009));
#24230=DIRECTION('ref_axis',(0.998867339183009,-1.22321929018916E-16,0.047581915823728));
#24231=DIRECTION('center_axis',(0.923227637511546,-1.13059043092106E-16,
-0.384253470166307));
#24232=DIRECTION('ref_axis',(-0.384253470166307,4.70559241043957E-17,-0.923227637511546));
#24233=DIRECTION('',(-1.22460635382238E-16,-1.,-2.46519032881566E-32));
#24234=DIRECTION('center_axis',(-0.128840552099425,1.57778958730938E-17,
0.991665322644044));
#24235=DIRECTION('ref_axis',(0.991665322644044,-1.21439965497521E-16,0.128840552099425));
#24236=DIRECTION('center_axis',(0.951475898762374,-1.16518343113326E-16,
-0.307723275158594));
#24237=DIRECTION('ref_axis',(-0.307723275158594,3.76839877978246E-17,-0.951475898762374));
#24238=DIRECTION('',(-1.22460635382238E-16,-1.,-2.46519032881566E-32));
#24239=DIRECTION('center_axis',(-0.209241775758096,2.56238808078441E-17,
0.977863936996144));
#24240=DIRECTION('ref_axis',(0.977863936996144,-1.19749839041924E-16,0.209241775758096));
#24241=DIRECTION('center_axis',(0.973392244889412,-1.192022327853E-16,-0.229145232525468));
#24242=DIRECTION('ref_axis',(-0.229145232525468,2.80612707698795E-17,-0.973392244889412));
#24243=DIRECTION('',(-1.22460635382238E-16,-1.,-2.46519032881566E-32));
#24244=DIRECTION('center_axis',(-0.288250529921558,3.52993430434607E-17,
0.957555028183728));
#24245=DIRECTION('ref_axis',(0.957555028183729,-1.17262797164836E-16,0.288250529921558));
#24246=DIRECTION('center_axis',(0.988830826225127,-1.21092851265072E-16,
-0.149042266176187));
#24247=DIRECTION('ref_axis',(-0.149042266176187,1.82518106147445E-17,-0.988830826225127));
#24248=DIRECTION('',(-1.22460635382238E-16,-1.,-2.46519032881566E-32));
#24249=DIRECTION('center_axis',(-0.365341024366383,4.47398939751048E-17,
0.930873748644209));
#24250=DIRECTION('ref_axis',(0.930873748644209,-1.13995390719615E-16,0.365341024366383));
#24251=DIRECTION('center_axis',(0.997688901557916,-1.22177616798589E-16,
-0.0679474481357467));
#24252=DIRECTION('ref_axis',(-0.0679474481357467,8.32088767130521E-18,-0.997688901557916));
#24253=DIRECTION('',(-1.22460635382238E-16,-1.,-2.46519032881566E-32));
#24254=DIRECTION('center_axis',(-0.440000234571075,5.38827082939075E-17,
0.89799765789082));
#24255=DIRECTION('ref_axis',(0.89799765789082,-1.09969363757071E-16,0.440000234571075));
#24256=DIRECTION('center_axis',(0.999907521857919,-1.22449310450199E-16,
0.0135995489614973));
#24257=DIRECTION('ref_axis',(0.0135995489614973,-1.66540940673678E-18,-0.999907521857919));
#24258=DIRECTION('',(-1.22460635382238E-16,-1.,-2.46519032881566E-32));
#24259=DIRECTION('center_axis',(-0.511731315809626,6.26669420790353E-17,
0.859145540883353));
#24260=DIRECTION('ref_axis',(0.859145540883353,-1.05211508822392E-16,0.511731315809626));
#24261=DIRECTION('center_axis',(0.995471922573086,-1.21906124143478E-16,
0.0950560433041702));
#24262=DIRECTION('ref_axis',(0.0950560433041702,-1.16406234599502E-17,-0.995471922573086));
#24263=DIRECTION('',(-1.22460635382238E-16,-1.,-2.46519032881566E-32));
#24264=DIRECTION('center_axis',(-0.580056909571188,7.10341377039448E-17,
0.814575952050343));
#24265=DIRECTION('ref_axis',(0.814575952050343,-9.97534886551763E-17,0.580056909571188));
#24266=DIRECTION('center_axis',(0.984411621884836,-1.20551672693676E-16,
0.175879955361797));
#24267=DIRECTION('ref_axis',(0.175879955361797,-2.15383710846052E-17,-0.984411621884836));
#24268=DIRECTION('',(-1.22460635382238E-16,-1.,-2.46519032881566E-32));
#24269=DIRECTION('center_axis',(-0.644522320302207,7.89286128622424E-17,
0.76458549465201));
#24270=DIRECTION('ref_axis',(0.76458549465201,-9.36316254791277E-17,0.644522320302207));
#24271=DIRECTION('center_axis',(0.966800224269427,-1.18394969751724E-16,
0.255533415334641));
#24272=DIRECTION('ref_axis',(0.255533415334641,-3.12927844032734E-17,-0.966800224269427));
#24273=DIRECTION('',(-1.22460635382238E-16,-1.,-2.46519032881566E-32));
#24274=DIRECTION('center_axis',(-0.704698541330313,8.62978311242462E-17,
0.709506846934496));
#24275=DIRECTION('ref_axis',(0.709506846934496,-8.68866592836464E-17,0.704698541330313));
#24276=DIRECTION('center_axis',(0.942754930672314,-1.15450367819869E-16,
0.333486342588479));
#24277=DIRECTION('ref_axis',(0.333486342588479,-4.08389494046837E-17,-0.942754930672314));
#24278=DIRECTION('',(-1.22460635382238E-16,-1.,-2.46519032881566E-32));
#24279=DIRECTION('center_axis',(-0.76018510983294,9.3092751558258E-17,0.649706548211022));
#24280=DIRECTION('ref_axis',(0.649706548211022,-7.95634767059223E-17,0.76018510983294));
#24281=DIRECTION('center_axis',(0.912435758555192,-1.11737462738143E-16,
0.409219973253765));
#24282=DIRECTION('ref_axis',(0.409219973253765,-5.01133379357584E-17,-0.912435758555192));
#24283=DIRECTION('',(-1.22460635382238E-16,-1.,-2.46519032881566E-32));
#24284=DIRECTION('center_axis',(-0.810612771851345,9.92681550898726E-17,
0.585582559603238));
#24285=DIRECTION('ref_axis',(0.585582559603238,-7.17108123177697E-17,0.810612771851345));
#24286=DIRECTION('center_axis',(0.876044477006188,-1.07280963277278E-16,
0.48223031251359));
#24287=DIRECTION('ref_axis',(0.48223031251359,-5.90542304709892E-17,-0.876044477006188));
#24288=DIRECTION('',(-1.22460635382238E-16,-1.,-2.46519032881566E-32));
#24289=DIRECTION('center_axis',(-0.855645939614771,1.04782945427457E-16,
0.517561615675617));
#24290=DIRECTION('ref_axis',(0.517561615675617,-6.33809243050936E-17,0.855645939614771));
#24291=DIRECTION('center_axis',(0.833823263999873,-1.02110526705916E-16,
0.552031488606037));
#24292=DIRECTION('ref_axis',(0.552031488606037,-6.76021268456979E-17,-0.833823263999873));
#24293=DIRECTION('',(-1.22460635382238E-16,-1.,-2.46519032881566E-32));
#24294=DIRECTION('center_axis',(-0.894984924821705,1.0960042255119E-16,
0.44609638458733));
#24295=DIRECTION('ref_axis',(0.446096384587331,-5.46292466982836E-17,0.894984924821705));
#24296=DIRECTION('center_axis',(0.786053094742794,-9.62605614263769E-17,
0.618158986220596));
#24297=DIRECTION('ref_axis',(0.618158986220596,-7.57001422198142E-17,-0.786053094742795));
#24298=DIRECTION('',(-1.22460635382238E-16,-1.,-2.46519032881566E-32));
#24299=DIRECTION('center_axis',(-0.928367933016068,1.13688526945642E-16,
0.371662455660338));
#24300=DIRECTION('ref_axis',(0.371662455660338,-4.55140204678878E-17,0.928367933016068));
#24301=DIRECTION('center_axis',(0.733051871829834,-8.97699979924202E-17,
0.680172737770911));
#24302=DIRECTION('ref_axis',(0.680172737770911,-8.3294385637102E-17,-0.733051871829834));
#24303=DIRECTION('',(-1.22460635382238E-16,-1.,-2.46519032881566E-32));
#24304=DIRECTION('center_axis',(-0.955572805786137,1.17020052950558E-16,
0.294755174410915));
#24305=DIRECTION('ref_axis',(0.294755174410915,-3.6095905940563E-17,0.955572805786137));
#24306=DIRECTION('center_axis',(0.675172309654891,-8.2682030032831E-17,
0.737660051971963));
#24307=DIRECTION('ref_axis',(0.737660051971963,-9.03343186605811E-17,-0.675172309654891));
#24308=DIRECTION('',(-1.22460635382238E-16,-1.,-2.46519032881566E-32));
#24309=DIRECTION('center_axis',(-0.976418499192115,1.19572829810037E-16,
0.215886346106968));
#24310=DIRECTION('ref_axis',(0.215886346106968,-2.6437579114609E-17,0.976418499192115));
#24311=DIRECTION('center_axis',(0.612799587154786,-7.5043826804948E-17,
0.790238360232484));
#24312=DIRECTION('ref_axis',(0.790238360232484,-9.67730916974876E-17,-0.612799587154786));
#24313=DIRECTION('',(-1.22460635382238E-16,-1.,-2.46519032881566E-32));
#24314=DIRECTION('center_axis',(-0.990766288583682,1.21329869215259E-16,
0.135580829788419));
#24315=DIRECTION('ref_axis',(0.135580829788419,-1.66033145615408E-17,0.990766288583682));
#24316=DIRECTION('center_axis',(0.54634878450698,-6.69062192910381E-17,
0.837557762585809));
#24317=DIRECTION('ref_axis',(0.837557762585809,-1.02567855775584E-16,-0.54634878450698));
#24318=DIRECTION('',(-1.22460635382238E-16,-1.,-2.46519032881566E-32));
#24319=DIRECTION('center_axis',(-0.998520691789656,1.22279478358873E-16,
0.0543730454168903));
#24320=DIRECTION('ref_axis',(0.0543730454168903,-6.65855768941968E-18,0.998520691789656));
#24321=DIRECTION('center_axis',(0.476262120839485,-5.83233619264954E-17,
0.879303356216429));
#24322=DIRECTION('ref_axis',(0.879303356216429,-1.07680047695998E-16,-0.476262120839484));
#24323=DIRECTION('',(-1.22460635382238E-16,-1.,-2.46519032881566E-32));
#24324=DIRECTION('center_axis',(-0.999630104536087,1.22415337748702E-16,
-0.0271965826009666));
#24325=DIRECTION('ref_axis',(-0.0271965826009666,3.33051078553986E-18,0.999630104536087));
#24326=DIRECTION('center_axis',(0.40300601133552,-4.93523722110092E-17,
0.915197331086271));
#24327=DIRECTION('ref_axis',(0.915197331086272,-1.12075646664953E-16,-0.40300601133552));
#24328=DIRECTION('',(-1.22460635382238E-16,-1.,-2.46519032881566E-32));
#24329=DIRECTION('center_axis',(-0.994087143864189,1.21736543262923E-16,
-0.108585221848735));
#24330=DIRECTION('ref_axis',(-0.108585221848735,1.32974152607173E-17,0.994087143864189));
#24331=DIRECTION('center_axis',(0.327067963317431,-4.00529506010271E-17,
0.945000818714665));
#24332=DIRECTION('ref_axis',(0.945000818714665,-1.15725400696533E-16,-0.327067963317431));
#24333=DIRECTION('',(-1.22460635382238E-16,-1.,-2.46519032881566E-32));
#24334=DIRECTION('center_axis',(-0.981928697262709,1.20247612166844E-16,
-0.1892512443604));
#24335=DIRECTION('ref_axis',(-0.1892512443604,2.31758276312537E-17,0.981928697262709));
#24336=DIRECTION('center_axis',(0.248953331965879,-3.04869832130668E-17,
0.968515481808673));
#24337=DIRECTION('ref_axis',(0.968515481808673,-1.18605021279824E-16,-0.248953331965879));
#24338=DIRECTION('',(-1.22460635382238E-16,-1.,-2.46519032881566E-32));
#24339=DIRECTION('center_axis',(-0.963235677187776,1.17958453051255E-16,
-0.268657831065104));
#24340=DIRECTION('ref_axis',(-0.268657831065104,3.29000086926465E-17,0.963235677187776));
#24341=DIRECTION('center_axis',(0.169181957264503,-2.07181299818217E-17,
0.985584834165051));
#24342=DIRECTION('ref_axis',(0.985584834165051,-1.2069534501495E-16,-0.169181957264503));
#24343=DIRECTION('',(-1.22460635382238E-16,-1.,-2.46519032881566E-32));
#24344=DIRECTION('center_axis',(-0.938132482603859,1.14884299892385E-16,
-0.346276544229492));
#24345=DIRECTION('ref_axis',(-0.346276544229492,4.24052456243092E-17,0.93813248260386));
#24346=DIRECTION('center_axis',(0.0882847045505903,-1.08114010137985E-17,
0.996095282060112));
#24347=DIRECTION('ref_axis',(0.996095282060113,-1.21982461142331E-16,-0.0882847045505903));
#24348=DIRECTION('',(-1.22460635382238E-16,-1.,-2.46519032881566E-32));
#24349=DIRECTION('center_axis',(-0.906786171129178,1.11045610672306E-16,
-0.421590844123641));
#24350=DIRECTION('ref_axis',(-0.421590844123641,5.1628282642715E-17,0.906786171129178));
#24351=DIRECTION('center_axis',(0.00679993169384408,-8.32723955783986E-19,
0.999976880197217));
#24352=DIRECTION('ref_axis',(0.999976880197217,-1.22457804116499E-16,-0.00679993169384408));
#24353=DIRECTION('',(-1.22460635382238E-16,-1.,-2.46519032881566E-32));
#24354=DIRECTION('center_axis',(-0.86940534729482,1.06467931234439E-16,
-0.49409952650774));
#24355=DIRECTION('ref_axis',(-0.49409952650774,6.05077419582007E-17,0.86940534729482));
#24356=DIRECTION('center_axis',(-0.074730093586415,9.15149474276644E-18,
0.997203797181181));
#24357=DIRECTION('ref_axis',(0.997203797181181,-1.22118210608388E-16,0.074730093586415));
#24358=DIRECTION('',(-1.22460635382238E-16,-1.,-2.46519032881566E-32));
#24359=DIRECTION('center_axis',(-0.826238774316,1.01181725280179E-16,-0.563320058063614));
#24360=DIRECTION('ref_axis',(-0.563320058063614,6.89845322340292E-17,0.826238774316));
#24361=DIRECTION('center_axis',(-0.155762802423454,1.90748117536942E-17,
0.98779448742195));
#24362=DIRECTION('ref_axis',(0.98779448742195,-1.20965940556764E-16,0.155762802423454));
#24363=DIRECTION('',(-1.22460635382238E-16,-1.,-2.46519032881566E-32));
#24364=DIRECTION('center_axis',(-0.777573718613909,9.52221716379887E-17,
-0.628791787574343));
#24365=DIRECTION('ref_axis',(-0.628791787574343,7.7002241829487E-17,0.777573718613909));
#24366=DIRECTION('center_axis',(-0.235758935509419,2.88711890395234E-17,
0.971811568323544));
#24367=DIRECTION('ref_axis',(0.971811568323544,-1.1900866212871E-16,0.235758935509419));
#24368=DIRECTION('',(-1.22460635382238E-16,-1.,-2.46519032881566E-32));
#24369=DIRECTION('center_axis',(-0.723734038105076,8.86289301541003E-17,
-0.690079011482106));
#24370=DIRECTION('ref_axis',(-0.690079011482105,8.45075142100451E-17,0.723734038105076));
#24371=DIRECTION('center_axis',(-0.314186131777054,3.84754333257055E-17,
0.949361403575568));
#24372=DIRECTION('ref_axis',(0.949361403575568,-1.16259400689237E-16,0.314186131777054));
#24373=DIRECTION('',(-1.22460635382238E-16,-1.,-2.46519032881566E-32));
#24374=DIRECTION('center_axis',(-0.665078026980365,8.14458777627806E-17,
-0.746773873423478));
#24375=DIRECTION('ref_axis',(-0.746773873423478,9.14504030262939E-17,0.665078026980365));
#24376=DIRECTION('center_axis',(-0.390522471174776,4.78236299511047E-17,
0.920593395320402));
#24377=DIRECTION('ref_axis',(0.920593395320402,-1.12736452119628E-16,0.390522471174777));
#24378=DIRECTION('',(-1.22460635382238E-16,-1.,-2.46519032881566E-32));
#24379=DIRECTION('center_axis',(-0.60199603131625,7.37208164925735E-17,
-0.798499078446234));
#24380=DIRECTION('ref_axis',(-0.798499078446233,9.7784704498657E-17,0.60199603131625));
#24381=DIRECTION('center_axis',(-0.464259947958503,5.68535682095229E-17,
0.885698989906598));
#24382=DIRECTION('ref_axis',(0.885698989906598,-1.08463261061368E-16,0.464259947958503));
#24383=DIRECTION('',(-1.22460635382238E-16,-1.,-2.46519032881566E-32));
#24384=DIRECTION('center_axis',(-0.53490785138608,6.55051553516869E-17,
-0.844910403845004));
#24385=DIRECTION('ref_axis',(-0.844910403845004,1.03468264895922E-16,0.53490785138608));
#24386=DIRECTION('center_axis',(-0.534907851386066,6.55051553516852E-17,
0.844910403845013));
#24387=DIRECTION('ref_axis',(0.844910403845013,-1.03468264895923E-16,0.534907851386066));
#24388=DIRECTION('',(-1.22460635382238E-16,-1.,-2.46519032881566E-32));
#24389=DIRECTION('center_axis',(-0.464259947958518,5.68535682095247E-17,
-0.88569898990659));
#24390=DIRECTION('ref_axis',(-0.88569898990659,1.08463261061367E-16,0.464259947958518));
#24391=DIRECTION('center_axis',(-0.601996031316237,7.37208164925719E-17,
0.798499078446243));
#24392=DIRECTION('ref_axis',(0.798499078446244,-9.77847044986583E-17,0.601996031316237));
#24393=DIRECTION('',(-1.22460635382238E-16,-1.,-2.46519032881566E-32));
#24394=DIRECTION('center_axis',(-0.390522471174792,4.78236299511067E-17,
-0.920593395320395));
#24395=DIRECTION('ref_axis',(-0.920593395320395,1.12736452119627E-16,0.390522471174792));
#24396=DIRECTION('center_axis',(-0.665078026980353,8.1445877762779E-17,
0.746773873423489));
#24397=DIRECTION('ref_axis',(0.746773873423489,-9.14504030262952E-17,0.665078026980353));
#24398=DIRECTION('',(-1.22460635382238E-16,-1.,-2.46519032881566E-32));
#24399=DIRECTION('center_axis',(-0.31418613177707,3.84754333257075E-17,
-0.949361403575562));
#24400=DIRECTION('ref_axis',(-0.949361403575562,1.16259400689236E-16,0.31418613177707));
#24401=DIRECTION('center_axis',(-0.723734038105065,8.86289301540989E-17,
0.690079011482118));
#24402=DIRECTION('ref_axis',(0.690079011482118,-8.45075142100467E-17,0.723734038105065));
#24403=DIRECTION('',(-1.22460635382238E-16,-1.,-2.46519032881566E-32));
#24404=DIRECTION('center_axis',(-0.235758935509435,2.88711890395255E-17,
-0.97181156832354));
#24405=DIRECTION('ref_axis',(-0.97181156832354,1.1900866212871E-16,0.235758935509435));
#24406=DIRECTION('center_axis',(-0.777573718613899,9.52221716379874E-17,
0.628791787574355));
#24407=DIRECTION('ref_axis',(0.628791787574355,-7.70022418294886E-17,0.777573718613899));
#24408=DIRECTION('',(-1.22460635382238E-16,-1.,-2.46519032881566E-32));
#24409=DIRECTION('center_axis',(-0.15576280242347,1.90748117536962E-17,
-0.987794487421947));
#24410=DIRECTION('ref_axis',(-0.987794487421947,1.20965940556763E-16,0.15576280242347));
#24411=DIRECTION('center_axis',(-0.826238774315991,1.01181725280178E-16,
0.563320058063628));
#24412=DIRECTION('ref_axis',(0.563320058063628,-6.89845322340309E-17,0.826238774315991));
#24413=DIRECTION('',(-1.22460635382238E-16,-1.,-2.46519032881566E-32));
#24414=DIRECTION('center_axis',(-0.0747300935864316,9.15149474276852E-18,
-0.99720379718118));
#24415=DIRECTION('ref_axis',(-0.99720379718118,1.22118210608387E-16,0.0747300935864316));
#24416=DIRECTION('center_axis',(-0.869405347294812,1.06467931234438E-16,
0.494099526507755));
#24417=DIRECTION('ref_axis',(0.494099526507755,-6.05077419582025E-17,0.869405347294812));
#24418=DIRECTION('',(-1.22460635382238E-16,-1.,-2.46519032881566E-32));
#24419=DIRECTION('center_axis',(0.00679993169382737,-8.32723955781891E-19,
-0.999976880197217));
#24420=DIRECTION('ref_axis',(-0.999976880197217,1.22457804116499E-16,-0.00679993169382737));
#24421=DIRECTION('center_axis',(-0.906786171129171,1.11045610672305E-16,
0.421590844123656));
#24422=DIRECTION('ref_axis',(0.421590844123656,-5.16282826427169E-17,0.906786171129171));
#24423=DIRECTION('',(-1.22460635382238E-16,-1.,-2.46519032881566E-32));
#24424=DIRECTION('center_axis',(0.0882847045505736,-1.08114010137964E-17,
-0.996095282060114));
#24425=DIRECTION('ref_axis',(-0.996095282060114,1.21982461142331E-16,-0.0882847045505736));
#24426=DIRECTION('center_axis',(-0.938132482603854,1.14884299892384E-16,
0.346276544229508));
#24427=DIRECTION('ref_axis',(0.346276544229508,-4.24052456243111E-17,0.938132482603854));
#24428=DIRECTION('',(-1.22460635382238E-16,-1.,-2.46519032881566E-32));
#24429=DIRECTION('center_axis',(0.169181957264487,-2.07181299818196E-17,
-0.985584834165054));
#24430=DIRECTION('ref_axis',(-0.985584834165054,1.2069534501495E-16,-0.169181957264487));
#24431=DIRECTION('center_axis',(-0.963235677187772,1.17958453051255E-16,
0.26865783106512));
#24432=DIRECTION('ref_axis',(0.26865783106512,-3.29000086926485E-17,0.963235677187772));
#24433=DIRECTION('',(-1.22460635382238E-16,-1.,-2.46519032881566E-32));
#24434=DIRECTION('center_axis',(0.248953331965864,-3.04869832130648E-17,
-0.968515481808677));
#24435=DIRECTION('ref_axis',(-0.968515481808677,1.18605021279825E-16,-0.248953331965864));
#24436=DIRECTION('center_axis',(-0.981928697262705,1.20247612166844E-16,
0.189251244360416));
#24437=DIRECTION('ref_axis',(0.189251244360416,-2.31758276312558E-17,0.981928697262706));
#24438=DIRECTION('',(-1.22460635382238E-16,-1.,-2.46519032881566E-32));
#24439=DIRECTION('center_axis',(0.327067963317415,-4.00529506010251E-17,
-0.945000818714671));
#24440=DIRECTION('ref_axis',(-0.945000818714671,1.15725400696533E-16,-0.327067963317415));
#24441=DIRECTION('center_axis',(-0.994087143864187,1.21736543262922E-16,
0.108585221848752));
#24442=DIRECTION('ref_axis',(0.108585221848752,-1.32974152607194E-17,0.994087143864187));
#24443=DIRECTION('',(-1.22460635382238E-16,-1.,-2.46519032881566E-32));
#24444=DIRECTION('center_axis',(0.403006011335506,-4.93523722110073E-17,
-0.915197331086278));
#24445=DIRECTION('ref_axis',(-0.915197331086278,1.12075646664954E-16,-0.403006011335505));
#24446=DIRECTION('center_axis',(-0.999630104536087,1.22415337748702E-16,
0.0271965826009838));
#24447=DIRECTION('ref_axis',(0.0271965826009838,-3.33051078554201E-18,0.999630104536087));
#24448=DIRECTION('',(-1.22460635382238E-16,-1.,-2.46519032881566E-32));
#24449=DIRECTION('center_axis',(0.476262120839469,-5.83233619264935E-17,
-0.879303356216437));
#24450=DIRECTION('ref_axis',(-0.879303356216437,1.07680047695999E-16,-0.476262120839469));
#24451=DIRECTION('center_axis',(-0.998520691789657,1.22279478358873E-16,
-0.0543730454168737));
#24452=DIRECTION('ref_axis',(-0.0543730454168737,6.65855768941759E-18,0.998520691789657));
#24453=DIRECTION('',(-1.22460635382238E-16,-1.,-2.46519032881566E-32));
#24454=DIRECTION('center_axis',(0.546348784506966,-6.69062192910363E-17,
-0.837557762585818));
#24455=DIRECTION('ref_axis',(-0.837557762585818,1.02567855775585E-16,-0.546348784506966));
#24456=DIRECTION('center_axis',(-0.990766288583684,1.2132986921526E-16,
-0.135580829788402));
#24457=DIRECTION('ref_axis',(-0.135580829788402,1.66033145615388E-17,0.990766288583684));
#24458=DIRECTION('',(-1.22460635382238E-16,-1.,-2.46519032881566E-32));
#24459=DIRECTION('center_axis',(0.612799587154772,-7.50438268049464E-17,
-0.790238360232494));
#24460=DIRECTION('ref_axis',(-0.790238360232494,9.67730916974889E-17,-0.612799587154772));
#24461=DIRECTION('center_axis',(-0.976418499192119,1.19572829810038E-16,
-0.215886346106952));
#24462=DIRECTION('ref_axis',(-0.215886346106952,2.6437579114607E-17,0.976418499192119));
#24463=DIRECTION('',(-1.22460635382238E-16,-1.,-2.46519032881566E-32));
#24464=DIRECTION('center_axis',(0.675172309654879,-8.26820300328295E-17,
-0.737660051971974));
#24465=DIRECTION('ref_axis',(-0.737660051971974,9.03343186605825E-17,-0.675172309654879));
#24466=DIRECTION('center_axis',(-0.955572805786142,1.17020052950559E-16,
-0.294755174410899));
#24467=DIRECTION('ref_axis',(-0.294755174410899,3.6095905940561E-17,0.955572805786142));
#24468=DIRECTION('',(-1.22460635382238E-16,-1.,-2.46519032881566E-32));
#24469=DIRECTION('center_axis',(0.733051871829822,-8.97699979924187E-17,
-0.680172737770924));
#24470=DIRECTION('ref_axis',(-0.680172737770924,8.32943856371034E-17,-0.733051871829822));
#24471=DIRECTION('center_axis',(-0.928367933016075,1.13688526945643E-16,
-0.371662455660323));
#24472=DIRECTION('ref_axis',(-0.371662455660323,4.55140204678859E-17,0.928367933016075));
#24473=DIRECTION('',(-1.22460635382238E-16,-1.,-2.46519032881566E-32));
#24474=DIRECTION('center_axis',(0.786053094742784,-9.62605614263756E-17,
-0.618158986220609));
#24475=DIRECTION('ref_axis',(-0.618158986220609,7.57001422198158E-17,-0.786053094742784));
#24476=DIRECTION('center_axis',(-0.894984924821712,1.09600422551191E-16,
-0.446096384587316));
#24477=DIRECTION('ref_axis',(-0.446096384587316,5.46292466982817E-17,0.894984924821712));
#24478=DIRECTION('',(-1.22460635382238E-16,-1.,-2.46519032881566E-32));
#24479=DIRECTION('center_axis',(0.833823263999864,-1.02110526705915E-16,
-0.552031488606051));
#24480=DIRECTION('ref_axis',(-0.552031488606051,6.76021268456996E-17,-0.833823263999864));
#24481=DIRECTION('center_axis',(-0.85564593961478,1.04782945427458E-16,
-0.517561615675603));
#24482=DIRECTION('ref_axis',(-0.517561615675603,6.33809243050919E-17,0.85564593961478));
#24483=DIRECTION('',(-1.22460635382238E-16,-1.,-2.46519032881566E-32));
#24484=DIRECTION('center_axis',(0.87604447700618,-1.07280963277277E-16,
-0.482230312513604));
#24485=DIRECTION('ref_axis',(-0.482230312513604,5.9054230470991E-17,-0.87604447700618));
#24486=DIRECTION('center_axis',(-0.810612771851354,9.92681550898737E-17,
-0.585582559603225));
#24487=DIRECTION('ref_axis',(-0.585582559603225,7.1710812317768E-17,0.810612771851354));
#24488=DIRECTION('',(-1.22460635382238E-16,-1.,-2.46519032881566E-32));
#24489=DIRECTION('center_axis',(0.912435758555185,-1.11737462738142E-16,
-0.40921997325378));
#24490=DIRECTION('ref_axis',(-0.40921997325378,5.01133379357602E-17,-0.912435758555185));
#24491=DIRECTION('center_axis',(-0.760185109832951,9.30927515582594E-17,
-0.649706548211009));
#24492=DIRECTION('ref_axis',(-0.649706548211009,7.95634767059206E-17,0.760185109832951));
#24493=DIRECTION('',(-1.22460635382238E-16,-1.,-2.46519032881566E-32));
#24494=DIRECTION('center_axis',(0.942754930672308,-1.15450367819868E-16,
-0.333486342588495));
#24495=DIRECTION('ref_axis',(-0.333486342588495,4.08389494046857E-17,-0.942754930672308));
#24496=DIRECTION('center_axis',(-0.704698541330324,8.62978311242476E-17,
-0.709506846934484));
#24497=DIRECTION('ref_axis',(-0.709506846934484,8.6886659283645E-17,0.704698541330324));
#24498=DIRECTION('',(-1.22460635382238E-16,-1.,-2.46519032881566E-32));
#24499=DIRECTION('center_axis',(0.966800224269422,-1.18394969751723E-16,
-0.255533415334658));
#24500=DIRECTION('ref_axis',(-0.255533415334658,3.12927844032754E-17,-0.966800224269422));
#24501=DIRECTION('center_axis',(-0.64452232030222,7.8928612862244E-17,-0.764585494652));
#24502=DIRECTION('ref_axis',(-0.764585494652,9.36316254791264E-17,0.64452232030222));
#24503=DIRECTION('',(-1.22460635382238E-16,-1.,-2.46519032881566E-32));
#24504=DIRECTION('center_axis',(0.984411621884833,-1.20551672693676E-16,
-0.175879955361814));
#24505=DIRECTION('ref_axis',(-0.175879955361814,2.15383710846073E-17,-0.984411621884833));
#24506=DIRECTION('center_axis',(-0.580056909571201,7.10341377039466E-17,
-0.814575952050334));
#24507=DIRECTION('ref_axis',(-0.814575952050334,9.9753488655175E-17,0.580056909571201));
#24508=DIRECTION('',(-1.22460635382238E-16,-1.,-2.46519032881566E-32));
#24509=DIRECTION('center_axis',(0.995471922573084,-1.21906124143478E-16,
-0.0950560433041868));
#24510=DIRECTION('ref_axis',(-0.0950560433041868,1.16406234599522E-17,-0.995471922573084));
#24511=DIRECTION('center_axis',(-0.51173131580964,6.26669420790371E-17,
-0.859145540883344));
#24512=DIRECTION('ref_axis',(-0.859145540883344,1.05211508822391E-16,0.51173131580964));
#24513=DIRECTION('',(-1.22460635382238E-16,-1.,-2.46519032881566E-32));
#24514=DIRECTION('center_axis',(0.999907521857918,-1.22449310450199E-16,
-0.013599548961514));
#24515=DIRECTION('ref_axis',(-0.013599548961514,1.66540940673888E-18,-0.999907521857918));
#24516=DIRECTION('center_axis',(-0.44000023457109,5.38827082939094E-17,
-0.897997657890813));
#24517=DIRECTION('ref_axis',(-0.897997657890813,1.0996936375707E-16,0.44000023457109));
#24518=DIRECTION('',(-1.22460635382238E-16,-1.,-2.46519032881566E-32));
#24519=DIRECTION('center_axis',(0.997688901557917,-1.22177616798589E-16,
0.0679474481357302));
#24520=DIRECTION('ref_axis',(0.0679474481357302,-8.32088767130315E-18,-0.997688901557917));
#24521=DIRECTION('center_axis',(-0.365341024366398,4.47398939751067E-17,
-0.930873748644203));
#24522=DIRECTION('ref_axis',(-0.930873748644203,1.13995390719615E-16,0.365341024366398));
#24523=DIRECTION('',(-1.22460635382238E-16,-1.,-2.46519032881566E-32));
#24524=DIRECTION('center_axis',(0.988830826225129,-1.21092851265072E-16,
0.149042266176171));
#24525=DIRECTION('ref_axis',(0.149042266176171,-1.82518106147425E-17,-0.988830826225129));
#24526=DIRECTION('center_axis',(-0.288250529921574,3.52993430434627E-17,
-0.957555028183724));
#24527=DIRECTION('ref_axis',(-0.957555028183724,1.17262797164835E-16,0.288250529921574));
#24528=DIRECTION('',(-1.22460635382238E-16,-1.,-2.46519032881566E-32));
#24529=DIRECTION('center_axis',(0.973392244889416,-1.19202232785301E-16,
0.229145232525452));
#24530=DIRECTION('ref_axis',(0.229145232525452,-2.80612707698774E-17,-0.973392244889416));
#24531=DIRECTION('center_axis',(-0.209241775758112,2.56238808078461E-17,
-0.977863936996141));
#24532=DIRECTION('ref_axis',(-0.977863936996141,1.19749839041924E-16,0.209241775758112));
#24533=DIRECTION('',(-1.22460635382238E-16,-1.,-2.46519032881566E-32));
#24534=DIRECTION('center_axis',(0.951475898762379,-1.16518343113327E-16,
0.307723275158579));
#24535=DIRECTION('ref_axis',(0.307723275158579,-3.76839877978227E-17,-0.951475898762379));
#24536=DIRECTION('center_axis',(-0.128840552099442,1.5777895873096E-17,
-0.991665322644042));
#24537=DIRECTION('ref_axis',(-0.991665322644042,1.21439965497521E-16,0.128840552099442));
#24538=DIRECTION('',(-1.22460635382238E-16,-1.,-2.46519032881566E-32));
#24539=DIRECTION('center_axis',(0.923227637511553,-1.13059043092107E-16,
0.384253470166292));
#24540=DIRECTION('ref_axis',(0.384253470166292,-4.70559241043938E-17,-0.923227637511553));
#24541=DIRECTION('center_axis',(-0.0475819158237449,5.82691164447997E-18,
-0.998867339183008));
#24542=DIRECTION('ref_axis',(-0.998867339183008,1.22321929018916E-16,0.0475819158237449));
#24543=DIRECTION('',(-1.22460635382238E-16,-1.,-2.46519032881566E-32));
#24544=DIRECTION('center_axis',(0.888835448654925,-1.08847353792538E-16,
0.458226521727408));
#24545=DIRECTION('ref_axis',(0.458226521727408,-5.61147109997311E-17,-0.888835448654925));
#24546=DIRECTION('center_axis',(0.0339933702512953,-4.16284971975726E-18,
-0.999422058381222));
#24547=DIRECTION('ref_axis',(-0.999422058381222,1.22389860284388E-16,-0.0339933702512953));
#24548=DIRECTION('',(-1.22460635382238E-16,-1.,-2.46519032881566E-32));
#24549=DIRECTION('center_axis',(0.848528206535025,-1.0391130331203E-16,
0.529150151388483));
#24550=DIRECTION('ref_axis',(0.529150151388483,-6.48000637516409E-17,-0.848528206535025));
#24551=DIRECTION('center_axis',(0.115342436055824,-1.41249080059314E-17,
-0.993325788673942));
#24552=DIRECTION('ref_axis',(-0.993325788673942,1.21643307222573E-16,-0.115342436055824));
#24553=DIRECTION('',(-1.22460635382238E-16,-1.,-2.46519032881566E-32));
#24554=DIRECTION('center_axis',(0.802574149197934,-9.82837402521379E-17,
0.596552374095697));
#24555=DIRECTION('ref_axis',(0.596552374095697,-7.30541827705414E-17,-0.802574149197934));
#24556=DIRECTION('center_axis',(0.195923916978565,-2.39929673597718E-17,
-0.980619099730256));
#24557=DIRECTION('ref_axis',(-0.980619099730256,1.20087238020925E-16,-0.195923916978565));
#24558=DIRECTION('',(-1.22460635382238E-16,-1.,-2.46519032881566E-32));
#24559=DIRECTION('center_axis',(0.751279093313345,-9.20021151165437E-17,
0.659984639177518));
#24560=DIRECTION('ref_axis',(0.659984639177518,-8.08221382561957E-17,-0.751279093313345));
#24561=DIRECTION('center_axis',(0.275201556558983,-3.37013574743939E-17,
-0.961386552468627));
#24562=DIRECTION('ref_axis',(-0.961386552468627,1.17732008063247E-16,-0.275201556558983));
#24563=DIRECTION('',(-1.22460635382238E-16,-1.,-2.46519032881566E-32));
#24564=DIRECTION('center_axis',(0.694984399015081,-8.51082310841295E-17,
0.719024815375413));
#24565=DIRECTION('ref_axis',(0.719024815375413,-8.80522357464692E-17,-0.694984399015081));
#24566=DIRECTION('center_axis',(0.352647775185563,-4.31854706153565E-17,
-0.935756136317937));
#24567=DIRECTION('ref_axis',(-0.935756136317937,1.14593291016322E-16,-0.352647775185563));
#24568=DIRECTION('',(-1.22460635382238E-16,-1.,-2.46519032881566E-32));
#24569=DIRECTION('center_axis',(0.634064698205726,-7.76479658157201E-17,
0.773280000057729));
#24570=DIRECTION('ref_axis',(0.773280000057729,-9.46963601354463E-17,-0.634064698205726));
#24571=DIRECTION('',(0.,0.,1.));
#24572=DIRECTION('',(1.,0.,0.));
#24573=DIRECTION('',(-0.634017109593488,4.26900148990998E-22,-0.773319018738527));
#24574=DIRECTION('',(-0.773319018738527,-4.70422967936641E-22,0.634017109593488));
#24575=DIRECTION('',(0.94600985821244,1.07727022234467E-21,0.324137853643906));
#24576=DIRECTION('',(9.56706854046674E-22,-1.,5.31305137801972E-22));
#24577=DIRECTION('',(-0.0206130756965559,0.,0.999787527982985));
#24578=DIRECTION('',(0.999787527982985,0.,0.0206130756965559));
#24579=DIRECTION('',(0.,0.,1.));
#24580=DIRECTION('',(1.,0.,0.));
#24581=DIRECTION('',(0.960325417034359,9.29045991324782E-17,-0.278881862798184));
#24582=DIRECTION('',(-0.245643287779639,-0.473460863973698,-0.845868893773786));
#24583=DIRECTION('',(4.58919400736298E-16,-1.,4.15300572011656E-16));
#24584=DIRECTION('',(-0.357727621945708,2.23650315000115E-16,0.933825973346784));
#24585=DIRECTION('',(0.757089833520179,0.445542247675854,0.477814911358295));
#24586=DIRECTION('',(0.51938165271092,-0.854131075843084,-0.026510452776398));
#24587=DIRECTION('',(-0.643067400011131,-0.370230816657486,-0.670368153658909));
#24588=DIRECTION('',(0.519381652710921,-0.854131075843083,-0.026510452776397));
#24589=DIRECTION('',(0.498609418850897,-0.614964651282495,0.610906805581809));
#24590=DIRECTION('',(0.738425973382313,-0.0677812250859528,-0.670919359804315));
#24591=DIRECTION('',(0.643067400011132,0.370230816657482,0.67036815365891));
#24592=DIRECTION('',(0.738425973382313,-0.0677812250859528,-0.670919359804314));
#24593=DIRECTION('',(-0.57791705675935,-0.339743616933039,0.742014925901001));
#24594=DIRECTION('',(-0.643067400011132,-0.370230816657483,-0.67036815365891));
#24595=DIRECTION('',(-0.622907115670884,0.762089648289778,0.176652464506279));
#24596=DIRECTION('',(0.643067400011132,0.370230816657483,0.670368153658911));
#24597=DIRECTION('',(-0.218718306406631,-0.932896284343021,0.28612379331611));
#24598=DIRECTION('',(0.414017075821557,0.176800571431943,0.892934162673545));
#24599=CARTESIAN_POINT('',(0.,0.,0.));
#24600=CARTESIAN_POINT('',(0.,0.,0.));
#24601=CARTESIAN_POINT('Origin',(0.,27.,0.));
#24602=CARTESIAN_POINT('',(-22.477766792989,27.,1.));
#24603=CARTESIAN_POINT('',(22.477766792989,27.,1.));
#24604=CARTESIAN_POINT('Origin',(0.,27.,0.));
#24605=CARTESIAN_POINT('',(22.477766792989,34.,1.));
#24606=CARTESIAN_POINT('',(22.477766792989,27.,1.));
#24607=CARTESIAN_POINT('',(-22.477766792989,34.,1.));
#24608=CARTESIAN_POINT('Origin',(0.,34.,0.));
#24609=CARTESIAN_POINT('',(-22.477766792989,27.,1.));
#24610=CARTESIAN_POINT('Origin',(0.,34.,0.));
#24611=CARTESIAN_POINT('',(24.9799919935936,5.,1.));
#24612=CARTESIAN_POINT('',(-24.9799919935936,5.,1.));
#24613=CARTESIAN_POINT('Origin',(0.,5.,0.));
#24614=CARTESIAN_POINT('',(24.9799919935936,27.,1.));
#24615=CARTESIAN_POINT('',(24.9799919935936,34.,1.));
#24616=CARTESIAN_POINT('',(-24.9799919935936,27.,1.));
#24617=CARTESIAN_POINT('Origin',(0.,27.,0.));
#24618=CARTESIAN_POINT('',(-24.9799919935936,34.,1.));
#24619=CARTESIAN_POINT('Origin',(-26.2146741366494,0.,1.));
#24620=CARTESIAN_POINT('',(22.477766792989,5.,1.));
#24621=CARTESIAN_POINT('',(-26.2146741366494,5.,1.));
#24622=CARTESIAN_POINT('',(22.477766792989,0.,1.));
#24623=CARTESIAN_POINT('',(22.477766792989,5.,1.));
#24624=CARTESIAN_POINT('',(10.4522724801834,0.,1.));
#24625=CARTESIAN_POINT('',(-26.2146741366494,0.,1.));
#24626=CARTESIAN_POINT('',(10.4522724801834,34.,1.));
#24627=CARTESIAN_POINT('',(10.4522724801834,34.,1.));
#24628=CARTESIAN_POINT('',(-26.2146741366494,34.,1.));
#24629=CARTESIAN_POINT('',(-26.2146741366494,27.,1.));
#24630=CARTESIAN_POINT('Origin',(-26.2146741366494,0.,1.));
#24631=CARTESIAN_POINT('',(-22.477766792989,5.,1.));
#24632=CARTESIAN_POINT('',(-26.2146741366494,5.,1.));
#24633=CARTESIAN_POINT('',(-26.2146741366494,27.,1.));
#24634=CARTESIAN_POINT('',(-10.4522724801834,34.,1.));
#24635=CARTESIAN_POINT('',(-26.2146741366494,34.,1.));
#24636=CARTESIAN_POINT('',(-10.4522724801834,0.,1.));
#24637=CARTESIAN_POINT('',(-10.4522724801834,34.,1.));
#24638=CARTESIAN_POINT('',(-22.477766792989,0.,1.));
#24639=CARTESIAN_POINT('',(-26.2146741366494,0.,1.));
#24640=CARTESIAN_POINT('',(-22.477766792989,5.,1.));
#24641=CARTESIAN_POINT('Origin',(0.,0.,0.));
#24642=CARTESIAN_POINT('Origin',(0.,0.,0.));
#24643=CARTESIAN_POINT('Origin',(0.,0.,0.));
#24644=CARTESIAN_POINT('Origin',(0.,34.,0.));
#24645=CARTESIAN_POINT('Origin',(0.,34.,0.));
#24646=CARTESIAN_POINT('Origin',(0.,34.,0.));
#24647=CARTESIAN_POINT('Origin',(0.,27.,0.));
#24648=CARTESIAN_POINT('Origin',(0.,5.,0.));
#24649=CARTESIAN_POINT('Origin',(0.,5.,0.));
#24650=CARTESIAN_POINT('Origin',(0.,5.,0.));
#24651=CARTESIAN_POINT('Origin',(0.,5.,0.));
#24652=CARTESIAN_POINT('',(-22.477766792989,5.,-1.));
#24653=CARTESIAN_POINT('',(22.477766792989,5.,-1.));
#24654=CARTESIAN_POINT('Origin',(0.,5.,0.));
#24655=CARTESIAN_POINT('',(22.477766792989,0.,-1.));
#24656=CARTESIAN_POINT('',(22.477766792989,5.,-1.));
#24657=CARTESIAN_POINT('',(-22.477766792989,0.,-1.));
#24658=CARTESIAN_POINT('Origin',(0.,0.,0.));
#24659=CARTESIAN_POINT('',(-22.477766792989,5.,-1.));
#24660=CARTESIAN_POINT('Origin',(0.,34.,0.));
#24661=CARTESIAN_POINT('',(10.4522724801834,34.,-1.));
#24662=CARTESIAN_POINT('',(-10.4522724801834,34.,-1.));
#24663=CARTESIAN_POINT('Origin',(0.,34.,0.));
#24664=CARTESIAN_POINT('',(-10.4522724801834,0.,-1.));
#24665=CARTESIAN_POINT('',(-10.4522724801834,34.,-1.));
#24666=CARTESIAN_POINT('',(10.4522724801834,0.,-1.));
#24667=CARTESIAN_POINT('Origin',(0.,0.,0.));
#24668=CARTESIAN_POINT('',(10.4522724801834,34.,-1.));
#24669=CARTESIAN_POINT('Origin',(0.,34.,0.));
#24670=CARTESIAN_POINT('',(24.9799919935936,27.,-1.));
#24671=CARTESIAN_POINT('',(-24.9799919935936,27.,-1.));
#24672=CARTESIAN_POINT('Origin',(0.,27.,0.));
#24673=CARTESIAN_POINT('',(24.9799919935936,5.,-1.));
#24674=CARTESIAN_POINT('',(24.9799919935936,34.,-1.));
#24675=CARTESIAN_POINT('',(-24.9799919935936,5.,-1.));
#24676=CARTESIAN_POINT('Origin',(0.,5.,0.));
#24677=CARTESIAN_POINT('',(-24.9799919935936,34.,-1.));
#24678=CARTESIAN_POINT('Origin',(-26.2146741366494,0.,-1.));
#24679=CARTESIAN_POINT('',(-26.2146741366494,5.,-1.));
#24680=CARTESIAN_POINT('',(-26.2146741366494,0.,-1.));
#24681=CARTESIAN_POINT('',(-22.477766792989,34.,-1.));
#24682=CARTESIAN_POINT('',(-26.2146741366494,34.,-1.));
#24683=CARTESIAN_POINT('',(-22.477766792989,27.,-1.));
#24684=CARTESIAN_POINT('',(-22.477766792989,27.,-1.));
#24685=CARTESIAN_POINT('',(-26.2146741366494,27.,-1.));
#24686=CARTESIAN_POINT('Origin',(-26.2146741366494,0.,-1.));
#24687=CARTESIAN_POINT('',(-26.2146741366494,5.,-1.));
#24688=CARTESIAN_POINT('',(22.477766792989,27.,-1.));
#24689=CARTESIAN_POINT('',(-26.2146741366494,27.,-1.));
#24690=CARTESIAN_POINT('',(22.477766792989,34.,-1.));
#24691=CARTESIAN_POINT('',(22.477766792989,27.,-1.));
#24692=CARTESIAN_POINT('',(-26.2146741366494,34.,-1.));
#24693=CARTESIAN_POINT('',(-26.2146741366494,0.,-1.));
#24694=CARTESIAN_POINT('Origin',(0.,0.,0.));
#24695=CARTESIAN_POINT('Origin',(0.,34.,0.));
#24696=CARTESIAN_POINT('Origin',(0.,34.,0.));
#24697=CARTESIAN_POINT('Origin',(0.,27.,0.));
#24698=CARTESIAN_POINT('Origin',(0.,27.,0.));
#24699=CARTESIAN_POINT('Origin',(0.,27.,0.));
#24700=CARTESIAN_POINT('Origin',(0.,5.,0.));
#24701=CARTESIAN_POINT('Origin',(24.9799919935936,0.,-1.));
#24702=CARTESIAN_POINT('',(24.9799919935936,5.,1.));
#24703=CARTESIAN_POINT('',(24.9799919935936,27.,1.));
#24704=CARTESIAN_POINT('',(24.9799919935936,0.,1.));
#24705=CARTESIAN_POINT('',(24.9799919935936,5.,-1.));
#24706=CARTESIAN_POINT('',(24.9799919935936,5.,-1.));
#24707=CARTESIAN_POINT('',(24.9799919935936,27.,-1.));
#24708=CARTESIAN_POINT('',(24.9799919935936,0.,-1.));
#24709=CARTESIAN_POINT('',(24.9799919935936,27.,-1.));
#24710=CARTESIAN_POINT('Origin',(10.4522724801834,0.,1.));
#24711=CARTESIAN_POINT('',(22.477766792989,0.,1.));
#24712=CARTESIAN_POINT('',(22.477766792989,5.,1.));
#24713=CARTESIAN_POINT('',(22.477766792989,5.,1.));
#24714=CARTESIAN_POINT('',(10.4522724801834,5.,1.));
#24715=CARTESIAN_POINT('',(22.477766792989,27.,1.));
#24716=CARTESIAN_POINT('',(10.4522724801834,27.,1.));
#24717=CARTESIAN_POINT('',(22.477766792989,34.,1.));
#24718=CARTESIAN_POINT('',(22.477766792989,27.,1.));
#24719=CARTESIAN_POINT('',(10.4522724801834,34.,1.));
#24720=CARTESIAN_POINT('',(10.4522724801834,34.,1.));
#24721=CARTESIAN_POINT('',(10.4522724801834,0.,1.));
#24722=CARTESIAN_POINT('',(10.4522724801834,0.,1.));
#24723=CARTESIAN_POINT('',(10.4522724801834,0.,1.));
#24724=CARTESIAN_POINT('Origin',(10.4522724801834,0.,-1.));
#24725=CARTESIAN_POINT('',(22.477766792989,5.,-1.));
#24726=CARTESIAN_POINT('',(10.4522724801834,5.,-1.));
#24727=CARTESIAN_POINT('',(22.477766792989,0.,-1.));
#24728=CARTESIAN_POINT('',(22.477766792989,5.,-1.));
#24729=CARTESIAN_POINT('',(10.4522724801834,0.,-1.));
#24730=CARTESIAN_POINT('',(10.4522724801834,0.,-1.));
#24731=CARTESIAN_POINT('',(10.4522724801834,34.,-1.));
#24732=CARTESIAN_POINT('',(10.4522724801834,0.,-1.));
#24733=CARTESIAN_POINT('',(22.477766792989,34.,-1.));
#24734=CARTESIAN_POINT('',(10.4522724801834,34.,-1.));
#24735=CARTESIAN_POINT('',(22.477766792989,27.,-1.));
#24736=CARTESIAN_POINT('',(22.477766792989,27.,-1.));
#24737=CARTESIAN_POINT('',(10.4522724801834,27.,-1.));
#24738=CARTESIAN_POINT('Origin',(-3.46944695195361E-15,0.,2.16840434497101E-16));
#24739=CARTESIAN_POINT('Origin',(0.,0.,0.));
#24740=CARTESIAN_POINT('Origin',(-3.46944695195361E-15,0.,2.16840434497101E-16));
#24741=CARTESIAN_POINT('Origin',(-3.46944695195361E-15,34.,2.16840434497101E-16));
#24742=CARTESIAN_POINT('Origin',(0.,34.,0.));
#24743=CARTESIAN_POINT('Origin',(-3.46944695195361E-15,34.,2.16840434497101E-16));
#24744=CARTESIAN_POINT('Origin',(-3.46944695195361E-15,0.,2.16840434497101E-16));
#24745=CARTESIAN_POINT('Origin',(0.,27.,0.));
#24746=CARTESIAN_POINT('Origin',(0.,27.,0.));
#24747=CARTESIAN_POINT('Origin',(0.,27.,0.));
#24748=CARTESIAN_POINT('Origin',(0.,5.,0.));
#24749=CARTESIAN_POINT('Origin',(0.,5.,0.));
#24750=CARTESIAN_POINT('Origin',(0.,5.,0.));
#24751=CARTESIAN_POINT('Origin',(-24.9799919935936,0.,-1.));
#24752=CARTESIAN_POINT('',(-24.9799919935936,5.,-1.));
#24753=CARTESIAN_POINT('',(-24.9799919935936,27.,-1.));
#24754=CARTESIAN_POINT('',(-24.9799919935936,0.,-1.));
#24755=CARTESIAN_POINT('',(-24.9799919935936,5.,1.));
#24756=CARTESIAN_POINT('',(-24.9799919935936,5.,-1.));
#24757=CARTESIAN_POINT('',(-24.9799919935936,27.,1.));
#24758=CARTESIAN_POINT('',(-24.9799919935936,0.,1.));
#24759=CARTESIAN_POINT('',(-24.9799919935936,27.,-1.));
#24760=CARTESIAN_POINT('Origin',(-24.9799919935936,0.,-1.));
#24761=CARTESIAN_POINT('',(-22.477766792989,0.,-1.));
#24762=CARTESIAN_POINT('',(-22.477766792989,5.,-1.));
#24763=CARTESIAN_POINT('',(-22.477766792989,5.,-1.));
#24764=CARTESIAN_POINT('',(-24.9799919935936,5.,-1.));
#24765=CARTESIAN_POINT('',(-22.477766792989,27.,-1.));
#24766=CARTESIAN_POINT('',(-24.9799919935936,27.,-1.));
#24767=CARTESIAN_POINT('',(-22.477766792989,34.,-1.));
#24768=CARTESIAN_POINT('',(-22.477766792989,27.,-1.));
#24769=CARTESIAN_POINT('',(-10.4522724801834,34.,-1.));
#24770=CARTESIAN_POINT('',(-24.9799919935936,34.,-1.));
#24771=CARTESIAN_POINT('',(-10.4522724801834,0.,-1.));
#24772=CARTESIAN_POINT('',(-10.4522724801834,0.,-1.));
#24773=CARTESIAN_POINT('',(-24.9799919935936,0.,-1.));
#24774=CARTESIAN_POINT('Origin',(-24.9799919935936,0.,1.));
#24775=CARTESIAN_POINT('',(-22.477766792989,5.,1.));
#24776=CARTESIAN_POINT('',(-24.9799919935936,5.,1.));
#24777=CARTESIAN_POINT('',(-22.477766792989,0.,1.));
#24778=CARTESIAN_POINT('',(-22.477766792989,5.,1.));
#24779=CARTESIAN_POINT('',(-10.4522724801834,0.,0.999999999999992));
#24780=CARTESIAN_POINT('',(-24.9799919935936,0.,1.));
#24781=CARTESIAN_POINT('',(-10.4522724801834,34.,0.999999999999992));
#24782=CARTESIAN_POINT('',(-10.4522724801834,0.,0.999999999999992));
#24783=CARTESIAN_POINT('',(-22.477766792989,34.,1.));
#24784=CARTESIAN_POINT('',(-24.9799919935936,34.,1.));
#24785=CARTESIAN_POINT('',(-22.477766792989,27.,1.));
#24786=CARTESIAN_POINT('',(-22.477766792989,27.,1.));
#24787=CARTESIAN_POINT('',(-24.9799919935936,27.,1.));
#24788=CARTESIAN_POINT('Origin',(-3.46944695195361E-15,0.,2.16840434497101E-16));
#24789=CARTESIAN_POINT('Origin',(0.,0.,0.));
#24790=CARTESIAN_POINT('Origin',(-3.46944695195361E-15,0.,2.16840434497101E-16));
#24791=CARTESIAN_POINT('Origin',(-3.46944695195361E-15,34.,2.16840434497101E-16));
#24792=CARTESIAN_POINT('Origin',(0.,34.,0.));
#24793=CARTESIAN_POINT('Origin',(-3.46944695195361E-15,34.,2.16840434497101E-16));
#24794=CARTESIAN_POINT('Origin',(-3.46944695195361E-15,0.,2.16840434497101E-16));
#24795=CARTESIAN_POINT('Origin',(0.,27.,0.));
#24796=CARTESIAN_POINT('Origin',(0.,27.,0.));
#24797=CARTESIAN_POINT('Origin',(0.,27.,0.));
#24798=CARTESIAN_POINT('Origin',(0.,5.,0.));
#24799=CARTESIAN_POINT('Origin',(0.,5.,0.));
#24800=CARTESIAN_POINT('Origin',(0.,5.,0.));
#24801=CARTESIAN_POINT('',(0.,0.,0.));
#24802=CARTESIAN_POINT('Origin',(0.,30.,0.));
#24803=CARTESIAN_POINT('',(9.9498743710662,2.,1.));
#24804=CARTESIAN_POINT('',(-9.9498743710662,2.,1.));
#24805=CARTESIAN_POINT('Origin',(0.,2.,0.));
#24806=CARTESIAN_POINT('',(9.94987437106619,30.,1.));
#24807=CARTESIAN_POINT('',(9.9498743710662,30.,1.));
#24808=CARTESIAN_POINT('',(-9.9498743710662,30.,1.));
#24809=CARTESIAN_POINT('Origin',(0.,30.,0.));
#24810=CARTESIAN_POINT('',(-9.9498743710662,30.,1.));
#24811=CARTESIAN_POINT('Origin',(0.,0.,0.));
#24812=CARTESIAN_POINT('',(7.93725393319377,0.,1.));
#24813=CARTESIAN_POINT('',(-7.93725393319377,0.,1.));
#24814=CARTESIAN_POINT('Origin',(0.,0.,0.));
#24815=CARTESIAN_POINT('',(0.,0.,1.));
#24816=CARTESIAN_POINT('Origin',(-10.8574973831368,0.,1.));
#24817=CARTESIAN_POINT('',(-7.93725393319377,2.,1.));
#24818=CARTESIAN_POINT('',(-10.8574973831368,2.,1.));
#24819=CARTESIAN_POINT('',(-10.8574973831368,30.,1.));
#24820=CARTESIAN_POINT('',(7.93725393319377,2.,1.));
#24821=CARTESIAN_POINT('',(-10.8574973831368,2.,1.));
#24822=CARTESIAN_POINT('',(7.93725393319377,2.,1.));
#24823=CARTESIAN_POINT('',(-7.93725393319377,2.,1.));
#24824=CARTESIAN_POINT('Origin',(0.,30.,0.));
#24825=CARTESIAN_POINT('Origin',(0.,2.,0.));
#24826=CARTESIAN_POINT('Origin',(0.,2.,0.));
#24827=CARTESIAN_POINT('Origin',(0.,2.,0.));
#24828=CARTESIAN_POINT('Origin',(0.,2.,0.));
#24829=CARTESIAN_POINT('',(-7.93725393319377,2.,-1.));
#24830=CARTESIAN_POINT('',(7.93725393319377,2.,-1.));
#24831=CARTESIAN_POINT('Origin',(0.,2.,0.));
#24832=CARTESIAN_POINT('',(7.93725393319377,0.,-1.));
#24833=CARTESIAN_POINT('',(7.93725393319377,2.,-1.));
#24834=CARTESIAN_POINT('',(-7.93725393319377,0.,-1.));
#24835=CARTESIAN_POINT('Origin',(0.,0.,0.));
#24836=CARTESIAN_POINT('',(-7.93725393319377,2.,-1.));
#24837=CARTESIAN_POINT('Origin',(0.,30.,0.));
#24838=CARTESIAN_POINT('',(9.94987437106619,30.,-1.));
#24839=CARTESIAN_POINT('',(-9.9498743710662,30.,-1.));
#24840=CARTESIAN_POINT('Origin',(0.,30.,0.));
#24841=CARTESIAN_POINT('',(9.9498743710662,2.,-1.));
#24842=CARTESIAN_POINT('',(9.9498743710662,30.,-1.));
#24843=CARTESIAN_POINT('',(-9.9498743710662,2.,-1.));
#24844=CARTESIAN_POINT('Origin',(0.,2.,0.));
#24845=CARTESIAN_POINT('',(-9.9498743710662,30.,-1.));
#24846=CARTESIAN_POINT('Origin',(0.,0.,0.));
#24847=CARTESIAN_POINT('',(0.,0.,-1.));
#24848=CARTESIAN_POINT('Origin',(-10.8574973831368,0.,-1.));
#24849=CARTESIAN_POINT('',(-10.8574973831368,2.,-1.));
#24850=CARTESIAN_POINT('',(-10.8574973831368,30.,-1.));
#24851=CARTESIAN_POINT('',(-10.8574973831368,2.,-1.));
#24852=CARTESIAN_POINT('Origin',(0.,30.,0.));
#24853=CARTESIAN_POINT('Origin',(0.,2.,0.));
#24854=CARTESIAN_POINT('Origin',(9.9498743710662,0.,1.));
#24855=CARTESIAN_POINT('',(9.9498743710662,2.,1.));
#24856=CARTESIAN_POINT('',(9.9498743710662,30.,1.));
#24857=CARTESIAN_POINT('',(9.9498743710662,0.,1.));
#24858=CARTESIAN_POINT('',(9.9498743710662,2.,-1.));
#24859=CARTESIAN_POINT('',(9.9498743710662,2.,1.));
#24860=CARTESIAN_POINT('',(9.9498743710662,30.,-1.));
#24861=CARTESIAN_POINT('',(9.9498743710662,0.,-1.));
#24862=CARTESIAN_POINT('',(9.9498743710662,30.,1.));
#24863=CARTESIAN_POINT('Origin',(-9.9498743710662,0.,1.));
#24864=CARTESIAN_POINT('',(-9.9498743710662,2.,1.));
#24865=CARTESIAN_POINT('',(-9.9498743710662,30.,1.));
#24866=CARTESIAN_POINT('',(-9.9498743710662,0.,1.));
#24867=CARTESIAN_POINT('',(-7.93725393319377,2.,1.));
#24868=CARTESIAN_POINT('',(-9.9498743710662,2.,1.));
#24869=CARTESIAN_POINT('',(-7.93725393319377,0.,1.));
#24870=CARTESIAN_POINT('',(-7.93725393319377,2.,1.));
#24871=CARTESIAN_POINT('',(7.93725393319377,0.,1.));
#24872=CARTESIAN_POINT('',(-9.9498743710662,0.,1.));
#24873=CARTESIAN_POINT('',(7.93725393319377,2.,1.));
#24874=CARTESIAN_POINT('',(7.93725393319377,2.,1.));
#24875=CARTESIAN_POINT('',(-9.9498743710662,2.,1.));
#24876=CARTESIAN_POINT('',(-9.9498743710662,30.,1.));
#24877=CARTESIAN_POINT('Origin',(-9.9498743710662,0.,1.));
#24878=CARTESIAN_POINT('',(-9.9498743710662,2.,-1.));
#24879=CARTESIAN_POINT('',(-9.9498743710662,30.,-1.));
#24880=CARTESIAN_POINT('',(-9.9498743710662,0.,-1.));
#24881=CARTESIAN_POINT('',(-9.9498743710662,2.,1.));
#24882=CARTESIAN_POINT('',(-9.9498743710662,30.,1.));
#24883=CARTESIAN_POINT('Origin',(-9.9498743710662,0.,-1.));
#24884=CARTESIAN_POINT('',(7.93725393319377,2.,-1.));
#24885=CARTESIAN_POINT('',(-9.9498743710662,2.,-1.));
#24886=CARTESIAN_POINT('',(7.93725393319377,0.,-1.));
#24887=CARTESIAN_POINT('',(7.93725393319377,2.,-1.));
#24888=CARTESIAN_POINT('',(-7.93725393319377,0.,-1.));
#24889=CARTESIAN_POINT('',(-9.9498743710662,0.,-1.));
#24890=CARTESIAN_POINT('',(-7.93725393319377,2.,-1.));
#24891=CARTESIAN_POINT('',(-7.93725393319377,2.,-1.));
#24892=CARTESIAN_POINT('',(-9.9498743710662,2.,-1.));
#24893=CARTESIAN_POINT('',(-9.9498743710662,30.,-1.));
#24894=CARTESIAN_POINT('Origin',(0.,0.,0.));
#24895=CARTESIAN_POINT('Origin',(0.,0.,0.));
#24896=CARTESIAN_POINT('Origin',(0.,0.,0.));
#24897=CARTESIAN_POINT('Origin',(0.,30.,0.));
#24898=CARTESIAN_POINT('Origin',(0.,2.,0.));
#24899=CARTESIAN_POINT('Origin',(0.,2.,0.));
#24900=CARTESIAN_POINT('Origin',(0.,2.,0.));
#24901=CARTESIAN_POINT('Origin',(0.,2.,0.));
#24902=CARTESIAN_POINT('Origin',(0.,2.,0.));
#24903=CARTESIAN_POINT('Origin',(0.,2.,0.));
#24904=CARTESIAN_POINT('Origin',(5.51672269044018,43.,2.35918858016532));
#24905=CARTESIAN_POINT('',(6.9531279684454,43.,2.97345743479371));
#24906=CARTESIAN_POINT('',(6.53903774184515,43.,-0.031391252358755));
#24907=CARTESIAN_POINT('',(6.53903774184515,43.,-0.0313912523587545));
#24908=CARTESIAN_POINT('Origin',(5.51672269044018,43.,2.35918858016532));
#24909=CARTESIAN_POINT('Origin',(-7.35563025392024,43.,-3.14558477355376));
#24910=CARTESIAN_POINT('',(-5.93400757601218,43.,-5.36540344129219));
#24911=CARTESIAN_POINT('',(-6.33331520251527,43.,-5.53616460607784));
#24912=CARTESIAN_POINT('Ctrl Pts',(-5.93400757601218,43.,-5.36540344129219));
#24913=CARTESIAN_POINT('Ctrl Pts',(-5.93400757601218,43.3291290637156,-5.36540344129219));
#24914=CARTESIAN_POINT('Ctrl Pts',(-5.98188388226438,43.6784012049209,-5.3138038536473));
#24915=CARTESIAN_POINT('Ctrl Pts',(-6.16344333601518,44.3181838212083,-5.10209873618755));
#24916=CARTESIAN_POINT('Ctrl Pts',(-6.29577793931752,44.6089260296629,-4.94153945058315));
#24917=CARTESIAN_POINT('Ctrl Pts',(-6.57591405287913,45.0679335530487,-4.56212012179661));
#24918=CARTESIAN_POINT('Ctrl Pts',(-6.74280768323277,45.2676678832806,-4.31723749028182));
#24919=CARTESIAN_POINT('Ctrl Pts',(-7.06842395635423,45.5337646559893,-3.76050232959795));
#24920=CARTESIAN_POINT('Ctrl Pts',(-7.22627127313154,45.6,-3.44807760118488));
#24921=CARTESIAN_POINT('Ctrl Pts',(-7.48498923470894,45.6,-2.84309194592264));
#24922=CARTESIAN_POINT('Ctrl Pts',(-7.60185005331357,45.5337646559893,-2.51313962298366));
#24923=CARTESIAN_POINT('Ctrl Pts',(-7.7794675367706,45.2676678832806,-1.89311379607514));
#24924=CARTESIAN_POINT('Ctrl Pts',(-7.84124260001151,45.0679335530487,-1.60327793108978));
#24925=CARTESIAN_POINT('Ctrl Pts',(-7.92206825557714,44.6089260296629,-1.13862485342795));
#24926=CARTESIAN_POINT('Ctrl Pts',(-7.94674595386654,44.3181838212083,-0.932026831578464));
#24927=CARTESIAN_POINT('Ctrl Pts',(-7.97440083953437,43.6784012049209,-0.654505482303069));
#24928=CARTESIAN_POINT('Ctrl Pts',(-7.97863767882213,43.3291290637156,-0.584243776244034));
#24929=CARTESIAN_POINT('Ctrl Pts',(-7.97863767882213,42.6708709362844,-0.584243776244034));
#24930=CARTESIAN_POINT('Ctrl Pts',(-7.97440083953437,42.3215987950791,-0.654505482303069));
#24931=CARTESIAN_POINT('Ctrl Pts',(-7.94674595386654,41.6818161787917,-0.932026831578464));
#24932=CARTESIAN_POINT('Ctrl Pts',(-7.92206825557714,41.3910739703371,-1.13862485342795));
#24933=CARTESIAN_POINT('Ctrl Pts',(-7.84124260001151,40.9320664469513,-1.60327793108978));
#24934=CARTESIAN_POINT('Ctrl Pts',(-7.7794675367706,40.7323321167194,-1.89311379607514));
#24935=CARTESIAN_POINT('Ctrl Pts',(-7.60185005331357,40.4662353440107,-2.51313962298366));
#24936=CARTESIAN_POINT('Ctrl Pts',(-7.48498923470894,40.4,-2.84309194592264));
#24937=CARTESIAN_POINT('Ctrl Pts',(-7.22627127313154,40.4,-3.44807760118488));
#24938=CARTESIAN_POINT('Ctrl Pts',(-7.06842395635423,40.4662353440107,-3.76050232959794));
#24939=CARTESIAN_POINT('Ctrl Pts',(-6.74280768323277,40.7323321167194,-4.31723749028181));
#24940=CARTESIAN_POINT('Ctrl Pts',(-6.57591405287913,40.9320664469513,-4.56212012179661));
#24941=CARTESIAN_POINT('Ctrl Pts',(-6.29577793931752,41.3910739703371,-4.94153945058315));
#24942=CARTESIAN_POINT('Ctrl Pts',(-6.16344333601518,41.6818161787917,-5.10209873618755));
#24943=CARTESIAN_POINT('Ctrl Pts',(-5.98188388226438,42.3215987950791,-5.3138038536473));
#24944=CARTESIAN_POINT('Ctrl Pts',(-5.93400757601218,42.6708709362844,-5.36540344129219));
#24945=CARTESIAN_POINT('Ctrl Pts',(-5.93400757601218,43.,-5.36540344129219));
#24946=CARTESIAN_POINT('Origin',(0.,48.,0.));
#24947=CARTESIAN_POINT('',(-9.79717439317883E-16,47.,8.));
#24948=CARTESIAN_POINT('Origin',(0.,47.,0.));
#24949=CARTESIAN_POINT('',(-8.57252759403147E-16,48.,7.));
#24950=CARTESIAN_POINT('',(-8.57252759403147E-16,48.,7.));
#24951=CARTESIAN_POINT('Origin',(0.,48.,0.));
#24952=CARTESIAN_POINT('Origin',(0.,32.,0.));
#24953=CARTESIAN_POINT('',(-1.20399315864541E-15,31.2588190451025,-9.66270045344786));
#24954=CARTESIAN_POINT('',(-1.18333951814346E-15,31.2588190451025,9.66270045344786));
#24955=CARTESIAN_POINT('Origin',(0.,31.2588190451025,0.));
#24956=CARTESIAN_POINT('Origin',(0.,31.2588190451025,0.));
#24957=CARTESIAN_POINT('',(-1.06504772100559E-15,32.,8.69677462715879));
#24958=CARTESIAN_POINT('',(-1.06504772100559E-15,32.,8.69677462715879));
#24959=CARTESIAN_POINT('Origin',(0.,32.,0.));
#24960=CARTESIAN_POINT('Origin',(0.,48.,0.));
#24961=CARTESIAN_POINT('',(-9.79717439317883E-16,32.,8.));
#24962=CARTESIAN_POINT('Origin',(0.,32.,0.));
#24963=CARTESIAN_POINT('',(-9.79717439317883E-16,48.,8.));
#24964=CARTESIAN_POINT('Origin',(0.,30.,0.));
#24965=CARTESIAN_POINT('',(1.22464679914735E-15,30.,-10.));
#24966=CARTESIAN_POINT('Origin',(0.,30.,0.));
#24967=CARTESIAN_POINT('',(1.22464679914735E-15,30.,-10.));
#24968=CARTESIAN_POINT('Origin',(0.,32.,0.));
#24969=CARTESIAN_POINT('Origin',(0.,30.,0.));
#24970=CARTESIAN_POINT('Origin',(0.,48.,0.));
#24971=CARTESIAN_POINT('',(0.,0.,0.));
#24972=CARTESIAN_POINT('Origin',(-43.8559375004335,-3.93782229046735E-15,
8.32667268468867E-14));
#24973=CARTESIAN_POINT('',(-43.6773437504336,-0.149957969249584,4.29423438922274));
#24974=CARTESIAN_POINT('',(-43.7170312504336,-0.149957969249584,4.29423438922274));
#24975=CARTESIAN_POINT('',(-43.8559375004333,-0.149957969249592,4.2942343892229));
#24976=CARTESIAN_POINT('',(-43.8757812504336,0.149957969249583,-4.29423438922274));
#24977=CARTESIAN_POINT('Ctrl Pts',(-43.8757812504336,0.149957969249583,
-4.29423438922274));
#24978=CARTESIAN_POINT('Ctrl Pts',(-43.8493229171003,2.62923534983068,-4.20765611530936));
#24979=CARTESIAN_POINT('Ctrl Pts',(-43.8228645837669,3.79389505549643,-2.0172497837413));
#24980=CARTESIAN_POINT('Ctrl Pts',(-43.7964062504336,4.95855476116219,0.173156547826753));
#24981=CARTESIAN_POINT('Ctrl Pts',(-43.7699479171003,3.64393708624685,2.27698460548143));
#24982=CARTESIAN_POINT('Ctrl Pts',(-43.7434895837669,2.32931941133151,4.38081266313611));
#24983=CARTESIAN_POINT('Ctrl Pts',(-43.7170312504336,-0.149957969249583,
4.29423438922274));
#24984=CARTESIAN_POINT('',(-43.8360937504336,0.149957969249583,-4.29423438922274));
#24985=CARTESIAN_POINT('',(-43.8559375004336,0.149957969249583,-4.29423438922274));
#24986=CARTESIAN_POINT('Ctrl Pts',(-43.8360937504336,0.149957969249583,
-4.29423438922274));
#24987=CARTESIAN_POINT('Ctrl Pts',(-43.8096354171003,2.62923534983068,-4.20765611530936));
#24988=CARTESIAN_POINT('Ctrl Pts',(-43.7831770837669,3.79389505549644,-2.0172497837413));
#24989=CARTESIAN_POINT('Ctrl Pts',(-43.7567187504336,4.95855476116219,0.173156547826753));
#24990=CARTESIAN_POINT('Ctrl Pts',(-43.7302604171003,3.64393708624685,2.27698460548143));
#24991=CARTESIAN_POINT('Ctrl Pts',(-43.7038020837669,2.32931941133151,4.38081266313611));
#24992=CARTESIAN_POINT('Ctrl Pts',(-43.6773437504336,-0.149957969249583,
4.29423438922274));
#24993=CARTESIAN_POINT('Origin',(-43.8559375004335,-3.93782229046735E-15,
8.32667268468867E-14));
#24994=CARTESIAN_POINT('',(-43.3598437504336,-0.149957969249584,4.29423438922274));
#24995=CARTESIAN_POINT('',(-43.3995312504336,-0.149957969249584,4.29423438922274));
#24996=CARTESIAN_POINT('',(-43.8559375004333,-0.149957969249592,4.2942343892229));
#24997=CARTESIAN_POINT('Ctrl Pts',(-43.7170312504336,-0.149957969249583,
4.29423438922274));
#24998=CARTESIAN_POINT('Ctrl Pts',(-43.6905729171003,-2.62923534983068,
4.20765611530936));
#24999=CARTESIAN_POINT('Ctrl Pts',(-43.6641145837669,-3.79389505549643,
2.01724978374131));
#25000=CARTESIAN_POINT('Ctrl Pts',(-43.6376562504336,-4.95855476116219,
-0.173156547826752));
#25001=CARTESIAN_POINT('Ctrl Pts',(-43.6111979171003,-3.64393708624685,
-2.27698460548143));
#25002=CARTESIAN_POINT('Ctrl Pts',(-43.5847395837669,-2.32931941133151,
-4.38081266313611));
#25003=CARTESIAN_POINT('Ctrl Pts',(-43.5582812504336,0.149957969249583,
-4.29423438922274));
#25004=CARTESIAN_POINT('Ctrl Pts',(-43.5318229171003,2.62923534983068,-4.20765611530936));
#25005=CARTESIAN_POINT('Ctrl Pts',(-43.5053645837669,3.79389505549643,-2.0172497837413));
#25006=CARTESIAN_POINT('Ctrl Pts',(-43.4789062504336,4.95855476116219,0.173156547826753));
#25007=CARTESIAN_POINT('Ctrl Pts',(-43.4524479171003,3.64393708624685,2.27698460548143));
#25008=CARTESIAN_POINT('Ctrl Pts',(-43.4259895837669,2.32931941133151,4.38081266313611));
#25009=CARTESIAN_POINT('Ctrl Pts',(-43.3995312504336,-0.149957969249583,
4.29423438922274));
#25010=CARTESIAN_POINT('Ctrl Pts',(-43.6773437504336,-0.149957969249583,
4.29423438922274));
#25011=CARTESIAN_POINT('Ctrl Pts',(-43.6508854171003,-2.62923534983068,
4.20765611530936));
#25012=CARTESIAN_POINT('Ctrl Pts',(-43.6244270837669,-3.79389505549643,
2.01724978374131));
#25013=CARTESIAN_POINT('Ctrl Pts',(-43.5979687504336,-4.95855476116219,
-0.173156547826752));
#25014=CARTESIAN_POINT('Ctrl Pts',(-43.5715104171003,-3.64393708624685,
-2.27698460548143));
#25015=CARTESIAN_POINT('Ctrl Pts',(-43.5450520837669,-2.32931941133151,
-4.38081266313611));
#25016=CARTESIAN_POINT('Ctrl Pts',(-43.5185937504336,0.149957969249583,
-4.29423438922274));
#25017=CARTESIAN_POINT('Ctrl Pts',(-43.4921354171003,2.62923534983068,-4.20765611530936));
#25018=CARTESIAN_POINT('Ctrl Pts',(-43.4656770837669,3.79389505549644,-2.0172497837413));
#25019=CARTESIAN_POINT('Ctrl Pts',(-43.4392187504336,4.95855476116219,0.173156547826753));
#25020=CARTESIAN_POINT('Ctrl Pts',(-43.4127604171003,3.64393708624685,2.27698460548143));
#25021=CARTESIAN_POINT('Ctrl Pts',(-43.3863020837669,2.32931941133151,4.38081266313611));
#25022=CARTESIAN_POINT('Ctrl Pts',(-43.3598437504336,-0.149957969249583,
4.29423438922274));
#25023=CARTESIAN_POINT('Origin',(-43.8559375004335,-3.93782229046735E-15,
8.32667268468867E-14));
#25024=CARTESIAN_POINT('',(-43.0423437504336,-0.149957969249583,4.29423438922274));
#25025=CARTESIAN_POINT('',(-43.0820312504336,-0.149957969249583,4.29423438922274));
#25026=CARTESIAN_POINT('',(-43.8559375004333,-0.149957969249592,4.2942343892229));
#25027=CARTESIAN_POINT('Ctrl Pts',(-43.3995312504336,-0.149957969249583,
4.29423438922274));
#25028=CARTESIAN_POINT('Ctrl Pts',(-43.3730729171003,-2.62923534983068,
4.20765611530936));
#25029=CARTESIAN_POINT('Ctrl Pts',(-43.3466145837669,-3.79389505549643,
2.01724978374131));
#25030=CARTESIAN_POINT('Ctrl Pts',(-43.3201562504336,-4.95855476116219,
-0.173156547826752));
#25031=CARTESIAN_POINT('Ctrl Pts',(-43.2936979171003,-3.64393708624685,
-2.27698460548143));
#25032=CARTESIAN_POINT('Ctrl Pts',(-43.2672395837669,-2.32931941133151,
-4.38081266313611));
#25033=CARTESIAN_POINT('Ctrl Pts',(-43.2407812504336,0.149957969249583,
-4.29423438922274));
#25034=CARTESIAN_POINT('Ctrl Pts',(-43.2143229171003,2.62923534983068,-4.20765611530936));
#25035=CARTESIAN_POINT('Ctrl Pts',(-43.1878645837669,3.79389505549643,-2.0172497837413));
#25036=CARTESIAN_POINT('Ctrl Pts',(-43.1614062504336,4.95855476116219,0.173156547826753));
#25037=CARTESIAN_POINT('Ctrl Pts',(-43.1349479171003,3.64393708624685,2.27698460548143));
#25038=CARTESIAN_POINT('Ctrl Pts',(-43.1084895837669,2.32931941133151,4.38081266313611));
#25039=CARTESIAN_POINT('Ctrl Pts',(-43.0820312504336,-0.149957969249583,
4.29423438922274));
#25040=CARTESIAN_POINT('Ctrl Pts',(-43.3598437504336,-0.149957969249583,
4.29423438922274));
#25041=CARTESIAN_POINT('Ctrl Pts',(-43.3333854171003,-2.62923534983068,
4.20765611530936));
#25042=CARTESIAN_POINT('Ctrl Pts',(-43.3069270837669,-3.79389505549643,
2.01724978374131));
#25043=CARTESIAN_POINT('Ctrl Pts',(-43.2804687504336,-4.95855476116219,
-0.173156547826752));
#25044=CARTESIAN_POINT('Ctrl Pts',(-43.2540104171003,-3.64393708624685,
-2.27698460548143));
#25045=CARTESIAN_POINT('Ctrl Pts',(-43.2275520837669,-2.32931941133151,
-4.38081266313611));
#25046=CARTESIAN_POINT('Ctrl Pts',(-43.2010937504336,0.149957969249583,
-4.29423438922274));
#25047=CARTESIAN_POINT('Ctrl Pts',(-43.1746354171003,2.62923534983068,-4.20765611530936));
#25048=CARTESIAN_POINT('Ctrl Pts',(-43.1481770837669,3.79389505549644,-2.0172497837413));
#25049=CARTESIAN_POINT('Ctrl Pts',(-43.1217187504336,4.95855476116219,0.173156547826753));
#25050=CARTESIAN_POINT('Ctrl Pts',(-43.0952604171003,3.64393708624685,2.27698460548143));
#25051=CARTESIAN_POINT('Ctrl Pts',(-43.0688020837669,2.32931941133151,4.38081266313611));
#25052=CARTESIAN_POINT('Ctrl Pts',(-43.0423437504336,-0.149957969249583,
4.29423438922274));
#25053=CARTESIAN_POINT('Origin',(-43.8559375004335,-3.93782229046735E-15,
8.32667268468867E-14));
#25054=CARTESIAN_POINT('',(-42.7248437504336,-0.149957969249583,4.29423438922274));
#25055=CARTESIAN_POINT('',(-42.7645312504336,-0.149957969249583,4.29423438922274));
#25056=CARTESIAN_POINT('',(-43.8559375004333,-0.149957969249592,4.2942343892229));
#25057=CARTESIAN_POINT('Ctrl Pts',(-43.0820312504336,-0.149957969249583,
4.29423438922274));
#25058=CARTESIAN_POINT('Ctrl Pts',(-43.0555729171003,-2.62923534983068,
4.20765611530936));
#25059=CARTESIAN_POINT('Ctrl Pts',(-43.0291145837669,-3.79389505549643,
2.01724978374131));
#25060=CARTESIAN_POINT('Ctrl Pts',(-43.0026562504336,-4.95855476116219,
-0.173156547826752));
#25061=CARTESIAN_POINT('Ctrl Pts',(-42.9761979171003,-3.64393708624685,
-2.27698460548143));
#25062=CARTESIAN_POINT('Ctrl Pts',(-42.9497395837669,-2.32931941133151,
-4.38081266313611));
#25063=CARTESIAN_POINT('Ctrl Pts',(-42.9232812504336,0.149957969249583,
-4.29423438922274));
#25064=CARTESIAN_POINT('Ctrl Pts',(-42.8968229171003,2.62923534983068,-4.20765611530936));
#25065=CARTESIAN_POINT('Ctrl Pts',(-42.8703645837669,3.79389505549643,-2.0172497837413));
#25066=CARTESIAN_POINT('Ctrl Pts',(-42.8439062504336,4.95855476116219,0.173156547826753));
#25067=CARTESIAN_POINT('Ctrl Pts',(-42.8174479171003,3.64393708624685,2.27698460548143));
#25068=CARTESIAN_POINT('Ctrl Pts',(-42.7909895837669,2.32931941133151,4.38081266313611));
#25069=CARTESIAN_POINT('Ctrl Pts',(-42.7645312504336,-0.149957969249583,
4.29423438922274));
#25070=CARTESIAN_POINT('Ctrl Pts',(-43.0423437504336,-0.149957969249583,
4.29423438922274));
#25071=CARTESIAN_POINT('Ctrl Pts',(-43.0158854171003,-2.62923534983068,
4.20765611530936));
#25072=CARTESIAN_POINT('Ctrl Pts',(-42.9894270837669,-3.79389505549643,
2.01724978374131));
#25073=CARTESIAN_POINT('Ctrl Pts',(-42.9629687504336,-4.95855476116219,
-0.173156547826752));
#25074=CARTESIAN_POINT('Ctrl Pts',(-42.9365104171003,-3.64393708624685,
-2.27698460548143));
#25075=CARTESIAN_POINT('Ctrl Pts',(-42.9100520837669,-2.32931941133151,
-4.38081266313611));
#25076=CARTESIAN_POINT('Ctrl Pts',(-42.8835937504336,0.149957969249583,
-4.29423438922274));
#25077=CARTESIAN_POINT('Ctrl Pts',(-42.8571354171003,2.62923534983068,-4.20765611530936));
#25078=CARTESIAN_POINT('Ctrl Pts',(-42.8306770837669,3.79389505549644,-2.0172497837413));
#25079=CARTESIAN_POINT('Ctrl Pts',(-42.8042187504336,4.95855476116219,0.173156547826753));
#25080=CARTESIAN_POINT('Ctrl Pts',(-42.7777604171003,3.64393708624685,2.27698460548143));
#25081=CARTESIAN_POINT('Ctrl Pts',(-42.7513020837669,2.32931941133151,4.38081266313611));
#25082=CARTESIAN_POINT('Ctrl Pts',(-42.7248437504336,-0.149957969249583,
4.29423438922274));
#25083=CARTESIAN_POINT('Origin',(-43.8559375004335,-3.93782229046735E-15,
8.32667268468867E-14));
#25084=CARTESIAN_POINT('',(-42.4073437504336,-0.149957969249582,4.29423438922274));
#25085=CARTESIAN_POINT('',(-42.4470312504336,-0.149957969249582,4.29423438922274));
#25086=CARTESIAN_POINT('',(-43.8559375004333,-0.149957969249592,4.2942343892229));
#25087=CARTESIAN_POINT('Ctrl Pts',(-42.7645312504336,-0.149957969249583,
4.29423438922274));
#25088=CARTESIAN_POINT('Ctrl Pts',(-42.7380729171003,-2.62923534983068,
4.20765611530936));
#25089=CARTESIAN_POINT('Ctrl Pts',(-42.7116145837669,-3.79389505549643,
2.01724978374131));
#25090=CARTESIAN_POINT('Ctrl Pts',(-42.6851562504336,-4.95855476116219,
-0.173156547826752));
#25091=CARTESIAN_POINT('Ctrl Pts',(-42.6586979171003,-3.64393708624685,
-2.27698460548143));
#25092=CARTESIAN_POINT('Ctrl Pts',(-42.6322395837669,-2.32931941133151,
-4.38081266313611));
#25093=CARTESIAN_POINT('Ctrl Pts',(-42.6057812504336,0.149957969249583,
-4.29423438922274));
#25094=CARTESIAN_POINT('Ctrl Pts',(-42.5793229171003,2.62923534983068,-4.20765611530936));
#25095=CARTESIAN_POINT('Ctrl Pts',(-42.5528645837669,3.79389505549643,-2.0172497837413));
#25096=CARTESIAN_POINT('Ctrl Pts',(-42.5264062504336,4.95855476116219,0.173156547826753));
#25097=CARTESIAN_POINT('Ctrl Pts',(-42.4999479171003,3.64393708624685,2.27698460548143));
#25098=CARTESIAN_POINT('Ctrl Pts',(-42.4734895837669,2.32931941133151,4.38081266313611));
#25099=CARTESIAN_POINT('Ctrl Pts',(-42.4470312504336,-0.149957969249583,
4.29423438922274));
#25100=CARTESIAN_POINT('Ctrl Pts',(-42.7248437504336,-0.149957969249583,
4.29423438922274));
#25101=CARTESIAN_POINT('Ctrl Pts',(-42.6983854171003,-2.62923534983068,
4.20765611530936));
#25102=CARTESIAN_POINT('Ctrl Pts',(-42.6719270837669,-3.79389505549643,
2.01724978374131));
#25103=CARTESIAN_POINT('Ctrl Pts',(-42.6454687504336,-4.95855476116219,
-0.173156547826752));
#25104=CARTESIAN_POINT('Ctrl Pts',(-42.6190104171003,-3.64393708624685,
-2.27698460548143));
#25105=CARTESIAN_POINT('Ctrl Pts',(-42.5925520837669,-2.32931941133151,
-4.38081266313611));
#25106=CARTESIAN_POINT('Ctrl Pts',(-42.5660937504336,0.149957969249583,
-4.29423438922274));
#25107=CARTESIAN_POINT('Ctrl Pts',(-42.5396354171003,2.62923534983068,-4.20765611530936));
#25108=CARTESIAN_POINT('Ctrl Pts',(-42.5131770837669,3.79389505549644,-2.0172497837413));
#25109=CARTESIAN_POINT('Ctrl Pts',(-42.4867187504336,4.95855476116219,0.173156547826753));
#25110=CARTESIAN_POINT('Ctrl Pts',(-42.4602604171003,3.64393708624685,2.27698460548143));
#25111=CARTESIAN_POINT('Ctrl Pts',(-42.4338020837669,2.32931941133151,4.38081266313611));
#25112=CARTESIAN_POINT('Ctrl Pts',(-42.4073437504336,-0.149957969249583,
4.29423438922274));
#25113=CARTESIAN_POINT('Origin',(-43.8559375004335,-3.93782229046735E-15,
8.32667268468867E-14));
#25114=CARTESIAN_POINT('',(-42.0898437504336,-0.149957969249582,4.29423438922274));
#25115=CARTESIAN_POINT('',(-42.1295312504336,-0.149957969249582,4.29423438922274));
#25116=CARTESIAN_POINT('',(-43.8559375004333,-0.149957969249592,4.2942343892229));
#25117=CARTESIAN_POINT('Ctrl Pts',(-42.4470312504336,-0.149957969249583,
4.29423438922274));
#25118=CARTESIAN_POINT('Ctrl Pts',(-42.4205729171003,-2.62923534983068,
4.20765611530936));
#25119=CARTESIAN_POINT('Ctrl Pts',(-42.3941145837669,-3.79389505549643,
2.01724978374131));
#25120=CARTESIAN_POINT('Ctrl Pts',(-42.3676562504336,-4.95855476116219,
-0.173156547826752));
#25121=CARTESIAN_POINT('Ctrl Pts',(-42.3411979171003,-3.64393708624685,
-2.27698460548143));
#25122=CARTESIAN_POINT('Ctrl Pts',(-42.3147395837669,-2.32931941133151,
-4.38081266313611));
#25123=CARTESIAN_POINT('Ctrl Pts',(-42.2882812504336,0.149957969249583,
-4.29423438922274));
#25124=CARTESIAN_POINT('Ctrl Pts',(-42.2618229171003,2.62923534983068,-4.20765611530936));
#25125=CARTESIAN_POINT('Ctrl Pts',(-42.2353645837669,3.79389505549643,-2.0172497837413));
#25126=CARTESIAN_POINT('Ctrl Pts',(-42.2089062504336,4.95855476116219,0.173156547826753));
#25127=CARTESIAN_POINT('Ctrl Pts',(-42.1824479171003,3.64393708624685,2.27698460548143));
#25128=CARTESIAN_POINT('Ctrl Pts',(-42.1559895837669,2.32931941133151,4.38081266313611));
#25129=CARTESIAN_POINT('Ctrl Pts',(-42.1295312504336,-0.149957969249583,
4.29423438922274));
#25130=CARTESIAN_POINT('Ctrl Pts',(-42.4073437504336,-0.149957969249583,
4.29423438922274));
#25131=CARTESIAN_POINT('Ctrl Pts',(-42.3808854171003,-2.62923534983068,
4.20765611530936));
#25132=CARTESIAN_POINT('Ctrl Pts',(-42.3544270837669,-3.79389505549643,
2.01724978374131));
#25133=CARTESIAN_POINT('Ctrl Pts',(-42.3279687504336,-4.95855476116219,
-0.173156547826752));
#25134=CARTESIAN_POINT('Ctrl Pts',(-42.3015104171003,-3.64393708624685,
-2.27698460548143));
#25135=CARTESIAN_POINT('Ctrl Pts',(-42.2750520837669,-2.32931941133151,
-4.38081266313611));
#25136=CARTESIAN_POINT('Ctrl Pts',(-42.2485937504336,0.149957969249583,
-4.29423438922274));
#25137=CARTESIAN_POINT('Ctrl Pts',(-42.2221354171003,2.62923534983068,-4.20765611530936));
#25138=CARTESIAN_POINT('Ctrl Pts',(-42.1956770837669,3.79389505549644,-2.0172497837413));
#25139=CARTESIAN_POINT('Ctrl Pts',(-42.1692187504336,4.95855476116219,0.173156547826753));
#25140=CARTESIAN_POINT('Ctrl Pts',(-42.1427604171003,3.64393708624685,2.27698460548143));
#25141=CARTESIAN_POINT('Ctrl Pts',(-42.1163020837669,2.32931941133151,4.38081266313611));
#25142=CARTESIAN_POINT('Ctrl Pts',(-42.0898437504336,-0.149957969249583,
4.29423438922274));
#25143=CARTESIAN_POINT('Origin',(-43.8559375004335,-3.93782229046735E-15,
8.32667268468867E-14));
#25144=CARTESIAN_POINT('',(-41.7723437504336,-0.149957969249581,4.29423438922274));
#25145=CARTESIAN_POINT('',(-41.8120312504336,-0.149957969249581,4.29423438922274));
#25146=CARTESIAN_POINT('',(-43.8559375004333,-0.149957969249592,4.2942343892229));
#25147=CARTESIAN_POINT('Ctrl Pts',(-42.1295312504336,-0.149957969249583,
4.29423438922274));
#25148=CARTESIAN_POINT('Ctrl Pts',(-42.1030729171003,-2.62923534983068,
4.20765611530936));
#25149=CARTESIAN_POINT('Ctrl Pts',(-42.0766145837669,-3.79389505549643,
2.01724978374131));
#25150=CARTESIAN_POINT('Ctrl Pts',(-42.0501562504336,-4.95855476116219,
-0.173156547826752));
#25151=CARTESIAN_POINT('Ctrl Pts',(-42.0236979171003,-3.64393708624685,
-2.27698460548143));
#25152=CARTESIAN_POINT('Ctrl Pts',(-41.9972395837669,-2.32931941133151,
-4.38081266313611));
#25153=CARTESIAN_POINT('Ctrl Pts',(-41.9707812504336,0.149957969249583,
-4.29423438922274));
#25154=CARTESIAN_POINT('Ctrl Pts',(-41.9443229171003,2.62923534983068,-4.20765611530936));
#25155=CARTESIAN_POINT('Ctrl Pts',(-41.9178645837669,3.79389505549643,-2.0172497837413));
#25156=CARTESIAN_POINT('Ctrl Pts',(-41.8914062504336,4.95855476116219,0.173156547826753));
#25157=CARTESIAN_POINT('Ctrl Pts',(-41.8649479171003,3.64393708624685,2.27698460548143));
#25158=CARTESIAN_POINT('Ctrl Pts',(-41.8384895837669,2.32931941133151,4.38081266313611));
#25159=CARTESIAN_POINT('Ctrl Pts',(-41.8120312504336,-0.149957969249583,
4.29423438922274));
#25160=CARTESIAN_POINT('Ctrl Pts',(-42.0898437504336,-0.149957969249583,
4.29423438922274));
#25161=CARTESIAN_POINT('Ctrl Pts',(-42.0633854171003,-2.62923534983068,
4.20765611530936));
#25162=CARTESIAN_POINT('Ctrl Pts',(-42.0369270837669,-3.79389505549643,
2.01724978374131));
#25163=CARTESIAN_POINT('Ctrl Pts',(-42.0104687504336,-4.95855476116219,
-0.173156547826752));
#25164=CARTESIAN_POINT('Ctrl Pts',(-41.9840104171003,-3.64393708624685,
-2.27698460548143));
#25165=CARTESIAN_POINT('Ctrl Pts',(-41.9575520837669,-2.32931941133151,
-4.38081266313611));
#25166=CARTESIAN_POINT('Ctrl Pts',(-41.9310937504336,0.149957969249583,
-4.29423438922274));
#25167=CARTESIAN_POINT('Ctrl Pts',(-41.9046354171003,2.62923534983068,-4.20765611530936));
#25168=CARTESIAN_POINT('Ctrl Pts',(-41.8781770837669,3.79389505549644,-2.0172497837413));
#25169=CARTESIAN_POINT('Ctrl Pts',(-41.8517187504336,4.95855476116219,0.173156547826753));
#25170=CARTESIAN_POINT('Ctrl Pts',(-41.8252604171003,3.64393708624685,2.27698460548143));
#25171=CARTESIAN_POINT('Ctrl Pts',(-41.7988020837669,2.32931941133151,4.38081266313611));
#25172=CARTESIAN_POINT('Ctrl Pts',(-41.7723437504336,-0.149957969249583,
4.29423438922274));
#25173=CARTESIAN_POINT('Origin',(-43.8559375004335,-3.93782229046735E-15,
8.32667268468867E-14));
#25174=CARTESIAN_POINT('',(-41.4548437504336,-0.149957969249581,4.29423438922274));
#25175=CARTESIAN_POINT('',(-41.4945312504336,-0.149957969249581,4.29423438922274));
#25176=CARTESIAN_POINT('',(-43.8559375004333,-0.149957969249592,4.2942343892229));
#25177=CARTESIAN_POINT('Ctrl Pts',(-41.8120312504336,-0.149957969249583,
4.29423438922274));
#25178=CARTESIAN_POINT('Ctrl Pts',(-41.7855729171003,-2.62923534983068,
4.20765611530936));
#25179=CARTESIAN_POINT('Ctrl Pts',(-41.7591145837669,-3.79389505549643,
2.01724978374131));
#25180=CARTESIAN_POINT('Ctrl Pts',(-41.7326562504336,-4.95855476116219,
-0.173156547826752));
#25181=CARTESIAN_POINT('Ctrl Pts',(-41.7061979171003,-3.64393708624685,
-2.27698460548143));
#25182=CARTESIAN_POINT('Ctrl Pts',(-41.6797395837669,-2.32931941133151,
-4.38081266313611));
#25183=CARTESIAN_POINT('Ctrl Pts',(-41.6532812504336,0.149957969249583,
-4.29423438922274));
#25184=CARTESIAN_POINT('Ctrl Pts',(-41.6268229171003,2.62923534983068,-4.20765611530936));
#25185=CARTESIAN_POINT('Ctrl Pts',(-41.6003645837669,3.79389505549643,-2.0172497837413));
#25186=CARTESIAN_POINT('Ctrl Pts',(-41.5739062504336,4.95855476116219,0.173156547826753));
#25187=CARTESIAN_POINT('Ctrl Pts',(-41.5474479171003,3.64393708624685,2.27698460548143));
#25188=CARTESIAN_POINT('Ctrl Pts',(-41.5209895837669,2.32931941133151,4.38081266313611));
#25189=CARTESIAN_POINT('Ctrl Pts',(-41.4945312504336,-0.149957969249583,
4.29423438922274));
#25190=CARTESIAN_POINT('Ctrl Pts',(-41.7723437504336,-0.149957969249583,
4.29423438922274));
#25191=CARTESIAN_POINT('Ctrl Pts',(-41.7458854171003,-2.62923534983068,
4.20765611530936));
#25192=CARTESIAN_POINT('Ctrl Pts',(-41.7194270837669,-3.79389505549643,
2.01724978374131));
#25193=CARTESIAN_POINT('Ctrl Pts',(-41.6929687504336,-4.95855476116219,
-0.173156547826752));
#25194=CARTESIAN_POINT('Ctrl Pts',(-41.6665104171003,-3.64393708624685,
-2.27698460548143));
#25195=CARTESIAN_POINT('Ctrl Pts',(-41.6400520837669,-2.32931941133151,
-4.38081266313611));
#25196=CARTESIAN_POINT('Ctrl Pts',(-41.6135937504336,0.149957969249583,
-4.29423438922274));
#25197=CARTESIAN_POINT('Ctrl Pts',(-41.5871354171003,2.62923534983068,-4.20765611530936));
#25198=CARTESIAN_POINT('Ctrl Pts',(-41.5606770837669,3.79389505549644,-2.0172497837413));
#25199=CARTESIAN_POINT('Ctrl Pts',(-41.5342187504336,4.95855476116219,0.173156547826753));
#25200=CARTESIAN_POINT('Ctrl Pts',(-41.5077604171003,3.64393708624685,2.27698460548143));
#25201=CARTESIAN_POINT('Ctrl Pts',(-41.4813020837669,2.32931941133151,4.38081266313611));
#25202=CARTESIAN_POINT('Ctrl Pts',(-41.4548437504336,-0.149957969249583,
4.29423438922274));
#25203=CARTESIAN_POINT('Origin',(-43.8559375004335,-3.93782229046735E-15,
8.32667268468867E-14));
#25204=CARTESIAN_POINT('',(-41.1373437504336,-0.14995796924958,4.29423438922274));
#25205=CARTESIAN_POINT('',(-41.1770312504336,-0.14995796924958,4.29423438922274));
#25206=CARTESIAN_POINT('',(-43.8559375004333,-0.149957969249592,4.2942343892229));
#25207=CARTESIAN_POINT('Ctrl Pts',(-41.4945312504336,-0.149957969249583,
4.29423438922274));
#25208=CARTESIAN_POINT('Ctrl Pts',(-41.4680729171003,-2.62923534983068,
4.20765611530936));
#25209=CARTESIAN_POINT('Ctrl Pts',(-41.4416145837669,-3.79389505549643,
2.01724978374131));
#25210=CARTESIAN_POINT('Ctrl Pts',(-41.4151562504336,-4.95855476116219,
-0.173156547826752));
#25211=CARTESIAN_POINT('Ctrl Pts',(-41.3886979171003,-3.64393708624685,
-2.27698460548143));
#25212=CARTESIAN_POINT('Ctrl Pts',(-41.3622395837669,-2.32931941133151,
-4.38081266313611));
#25213=CARTESIAN_POINT('Ctrl Pts',(-41.3357812504336,0.149957969249583,
-4.29423438922274));
#25214=CARTESIAN_POINT('Ctrl Pts',(-41.3093229171003,2.62923534983068,-4.20765611530936));
#25215=CARTESIAN_POINT('Ctrl Pts',(-41.2828645837669,3.79389505549643,-2.0172497837413));
#25216=CARTESIAN_POINT('Ctrl Pts',(-41.2564062504336,4.95855476116219,0.173156547826753));
#25217=CARTESIAN_POINT('Ctrl Pts',(-41.2299479171003,3.64393708624685,2.27698460548143));
#25218=CARTESIAN_POINT('Ctrl Pts',(-41.2034895837669,2.32931941133151,4.38081266313611));
#25219=CARTESIAN_POINT('Ctrl Pts',(-41.1770312504336,-0.149957969249583,
4.29423438922274));
#25220=CARTESIAN_POINT('Ctrl Pts',(-41.4548437504336,-0.149957969249583,
4.29423438922274));
#25221=CARTESIAN_POINT('Ctrl Pts',(-41.4283854171003,-2.62923534983068,
4.20765611530936));
#25222=CARTESIAN_POINT('Ctrl Pts',(-41.4019270837669,-3.79389505549643,
2.01724978374131));
#25223=CARTESIAN_POINT('Ctrl Pts',(-41.3754687504336,-4.95855476116219,
-0.173156547826752));
#25224=CARTESIAN_POINT('Ctrl Pts',(-41.3490104171003,-3.64393708624685,
-2.27698460548143));
#25225=CARTESIAN_POINT('Ctrl Pts',(-41.3225520837669,-2.32931941133151,
-4.38081266313611));
#25226=CARTESIAN_POINT('Ctrl Pts',(-41.2960937504336,0.149957969249583,
-4.29423438922274));
#25227=CARTESIAN_POINT('Ctrl Pts',(-41.2696354171003,2.62923534983068,-4.20765611530936));
#25228=CARTESIAN_POINT('Ctrl Pts',(-41.2431770837669,3.79389505549644,-2.0172497837413));
#25229=CARTESIAN_POINT('Ctrl Pts',(-41.2167187504336,4.95855476116219,0.173156547826753));
#25230=CARTESIAN_POINT('Ctrl Pts',(-41.1902604171003,3.64393708624685,2.27698460548143));
#25231=CARTESIAN_POINT('Ctrl Pts',(-41.1638020837669,2.32931941133151,4.38081266313611));
#25232=CARTESIAN_POINT('Ctrl Pts',(-41.1373437504336,-0.149957969249583,
4.29423438922274));
#25233=CARTESIAN_POINT('Origin',(-43.8559375004335,-3.93782229046735E-15,
8.32667268468867E-14));
#25234=CARTESIAN_POINT('',(-40.8198437504336,-0.14995796924958,4.29423438922274));
#25235=CARTESIAN_POINT('',(-40.8595312504336,-0.14995796924958,4.29423438922274));
#25236=CARTESIAN_POINT('',(-43.8559375004333,-0.149957969249592,4.2942343892229));
#25237=CARTESIAN_POINT('Ctrl Pts',(-41.1770312504336,-0.149957969249583,
4.29423438922274));
#25238=CARTESIAN_POINT('Ctrl Pts',(-41.1505729171003,-2.62923534983068,
4.20765611530936));
#25239=CARTESIAN_POINT('Ctrl Pts',(-41.1241145837669,-3.79389505549643,
2.01724978374131));
#25240=CARTESIAN_POINT('Ctrl Pts',(-41.0976562504336,-4.95855476116219,
-0.173156547826752));
#25241=CARTESIAN_POINT('Ctrl Pts',(-41.0711979171003,-3.64393708624685,
-2.27698460548143));
#25242=CARTESIAN_POINT('Ctrl Pts',(-41.0447395837669,-2.32931941133151,
-4.38081266313611));
#25243=CARTESIAN_POINT('Ctrl Pts',(-41.0182812504336,0.149957969249583,
-4.29423438922274));
#25244=CARTESIAN_POINT('Ctrl Pts',(-40.9918229171003,2.62923534983068,-4.20765611530936));
#25245=CARTESIAN_POINT('Ctrl Pts',(-40.9653645837669,3.79389505549643,-2.0172497837413));
#25246=CARTESIAN_POINT('Ctrl Pts',(-40.9389062504336,4.95855476116219,0.173156547826753));
#25247=CARTESIAN_POINT('Ctrl Pts',(-40.9124479171003,3.64393708624685,2.27698460548143));
#25248=CARTESIAN_POINT('Ctrl Pts',(-40.8859895837669,2.32931941133151,4.38081266313611));
#25249=CARTESIAN_POINT('Ctrl Pts',(-40.8595312504336,-0.149957969249583,
4.29423438922274));
#25250=CARTESIAN_POINT('Ctrl Pts',(-41.1373437504336,-0.149957969249583,
4.29423438922274));
#25251=CARTESIAN_POINT('Ctrl Pts',(-41.1108854171003,-2.62923534983068,
4.20765611530936));
#25252=CARTESIAN_POINT('Ctrl Pts',(-41.0844270837669,-3.79389505549643,
2.01724978374131));
#25253=CARTESIAN_POINT('Ctrl Pts',(-41.0579687504336,-4.95855476116219,
-0.173156547826752));
#25254=CARTESIAN_POINT('Ctrl Pts',(-41.0315104171003,-3.64393708624685,
-2.27698460548143));
#25255=CARTESIAN_POINT('Ctrl Pts',(-41.0050520837669,-2.32931941133151,
-4.38081266313611));
#25256=CARTESIAN_POINT('Ctrl Pts',(-40.9785937504336,0.149957969249583,
-4.29423438922274));
#25257=CARTESIAN_POINT('Ctrl Pts',(-40.9521354171003,2.62923534983068,-4.20765611530936));
#25258=CARTESIAN_POINT('Ctrl Pts',(-40.9256770837669,3.79389505549644,-2.0172497837413));
#25259=CARTESIAN_POINT('Ctrl Pts',(-40.8992187504336,4.95855476116219,0.173156547826753));
#25260=CARTESIAN_POINT('Ctrl Pts',(-40.8727604171003,3.64393708624685,2.27698460548143));
#25261=CARTESIAN_POINT('Ctrl Pts',(-40.8463020837669,2.32931941133151,4.38081266313611));
#25262=CARTESIAN_POINT('Ctrl Pts',(-40.8198437504336,-0.149957969249583,
4.29423438922274));
#25263=CARTESIAN_POINT('Origin',(-43.8559375004335,-3.93782229046735E-15,
8.32667268468867E-14));
#25264=CARTESIAN_POINT('',(-40.5023437504336,-0.149957969249579,4.29423438922274));
#25265=CARTESIAN_POINT('',(-40.5420312504336,-0.149957969249579,4.29423438922274));
#25266=CARTESIAN_POINT('',(-43.8559375004333,-0.149957969249592,4.2942343892229));
#25267=CARTESIAN_POINT('Ctrl Pts',(-40.8595312504336,-0.149957969249583,
4.29423438922274));
#25268=CARTESIAN_POINT('Ctrl Pts',(-40.8330729171003,-2.62923534983068,
4.20765611530936));
#25269=CARTESIAN_POINT('Ctrl Pts',(-40.8066145837669,-3.79389505549643,
2.01724978374131));
#25270=CARTESIAN_POINT('Ctrl Pts',(-40.7801562504336,-4.95855476116219,
-0.173156547826752));
#25271=CARTESIAN_POINT('Ctrl Pts',(-40.7536979171003,-3.64393708624685,
-2.27698460548143));
#25272=CARTESIAN_POINT('Ctrl Pts',(-40.7272395837669,-2.32931941133151,
-4.38081266313611));
#25273=CARTESIAN_POINT('Ctrl Pts',(-40.7007812504336,0.149957969249583,
-4.29423438922274));
#25274=CARTESIAN_POINT('Ctrl Pts',(-40.6743229171003,2.62923534983068,-4.20765611530936));
#25275=CARTESIAN_POINT('Ctrl Pts',(-40.6478645837669,3.79389505549643,-2.0172497837413));
#25276=CARTESIAN_POINT('Ctrl Pts',(-40.6214062504336,4.95855476116219,0.173156547826753));
#25277=CARTESIAN_POINT('Ctrl Pts',(-40.5949479171003,3.64393708624685,2.27698460548143));
#25278=CARTESIAN_POINT('Ctrl Pts',(-40.5684895837669,2.32931941133151,4.38081266313611));
#25279=CARTESIAN_POINT('Ctrl Pts',(-40.5420312504336,-0.149957969249583,
4.29423438922274));
#25280=CARTESIAN_POINT('Ctrl Pts',(-40.8198437504336,-0.149957969249583,
4.29423438922274));
#25281=CARTESIAN_POINT('Ctrl Pts',(-40.7933854171003,-2.62923534983068,
4.20765611530936));
#25282=CARTESIAN_POINT('Ctrl Pts',(-40.7669270837669,-3.79389505549643,
2.01724978374131));
#25283=CARTESIAN_POINT('Ctrl Pts',(-40.7404687504336,-4.95855476116219,
-0.173156547826752));
#25284=CARTESIAN_POINT('Ctrl Pts',(-40.7140104171003,-3.64393708624685,
-2.27698460548143));
#25285=CARTESIAN_POINT('Ctrl Pts',(-40.6875520837669,-2.32931941133151,
-4.38081266313611));
#25286=CARTESIAN_POINT('Ctrl Pts',(-40.6610937504336,0.149957969249583,
-4.29423438922274));
#25287=CARTESIAN_POINT('Ctrl Pts',(-40.6346354171003,2.62923534983068,-4.20765611530936));
#25288=CARTESIAN_POINT('Ctrl Pts',(-40.6081770837669,3.79389505549644,-2.0172497837413));
#25289=CARTESIAN_POINT('Ctrl Pts',(-40.5817187504336,4.95855476116219,0.173156547826753));
#25290=CARTESIAN_POINT('Ctrl Pts',(-40.5552604171002,3.64393708624685,2.27698460548143));
#25291=CARTESIAN_POINT('Ctrl Pts',(-40.5288020837669,2.32931941133151,4.38081266313611));
#25292=CARTESIAN_POINT('Ctrl Pts',(-40.5023437504336,-0.149957969249583,
4.29423438922274));
#25293=CARTESIAN_POINT('Origin',(-43.8559375004335,-3.93782229046735E-15,
8.32667268468867E-14));
#25294=CARTESIAN_POINT('',(-40.1848437504336,-0.149957969249579,4.29423438922274));
#25295=CARTESIAN_POINT('',(-40.2245312504336,-0.149957969249579,4.29423438922274));
#25296=CARTESIAN_POINT('',(-43.8559375004333,-0.149957969249592,4.2942343892229));
#25297=CARTESIAN_POINT('Ctrl Pts',(-40.5420312504336,-0.149957969249583,
4.29423438922274));
#25298=CARTESIAN_POINT('Ctrl Pts',(-40.5155729171003,-2.62923534983068,
4.20765611530936));
#25299=CARTESIAN_POINT('Ctrl Pts',(-40.4891145837669,-3.79389505549643,
2.01724978374131));
#25300=CARTESIAN_POINT('Ctrl Pts',(-40.4626562504336,-4.95855476116219,
-0.173156547826752));
#25301=CARTESIAN_POINT('Ctrl Pts',(-40.4361979171003,-3.64393708624685,
-2.27698460548143));
#25302=CARTESIAN_POINT('Ctrl Pts',(-40.4097395837669,-2.32931941133151,
-4.38081266313611));
#25303=CARTESIAN_POINT('Ctrl Pts',(-40.3832812504336,0.149957969249583,
-4.29423438922274));
#25304=CARTESIAN_POINT('Ctrl Pts',(-40.3568229171003,2.62923534983068,-4.20765611530936));
#25305=CARTESIAN_POINT('Ctrl Pts',(-40.3303645837669,3.79389505549643,-2.0172497837413));
#25306=CARTESIAN_POINT('Ctrl Pts',(-40.3039062504336,4.95855476116219,0.173156547826753));
#25307=CARTESIAN_POINT('Ctrl Pts',(-40.2774479171003,3.64393708624685,2.27698460548143));
#25308=CARTESIAN_POINT('Ctrl Pts',(-40.2509895837669,2.32931941133151,4.38081266313611));
#25309=CARTESIAN_POINT('Ctrl Pts',(-40.2245312504336,-0.149957969249583,
4.29423438922274));
#25310=CARTESIAN_POINT('Ctrl Pts',(-40.5023437504336,-0.149957969249583,
4.29423438922274));
#25311=CARTESIAN_POINT('Ctrl Pts',(-40.4758854171003,-2.62923534983068,
4.20765611530936));
#25312=CARTESIAN_POINT('Ctrl Pts',(-40.4494270837669,-3.79389505549643,
2.01724978374131));
#25313=CARTESIAN_POINT('Ctrl Pts',(-40.4229687504336,-4.95855476116219,
-0.173156547826752));
#25314=CARTESIAN_POINT('Ctrl Pts',(-40.3965104171003,-3.64393708624685,
-2.27698460548143));
#25315=CARTESIAN_POINT('Ctrl Pts',(-40.3700520837669,-2.32931941133151,
-4.38081266313611));
#25316=CARTESIAN_POINT('Ctrl Pts',(-40.3435937504336,0.149957969249583,
-4.29423438922274));
#25317=CARTESIAN_POINT('Ctrl Pts',(-40.3171354171003,2.62923534983068,-4.20765611530936));
#25318=CARTESIAN_POINT('Ctrl Pts',(-40.2906770837669,3.79389505549644,-2.0172497837413));
#25319=CARTESIAN_POINT('Ctrl Pts',(-40.2642187504336,4.95855476116219,0.173156547826753));
#25320=CARTESIAN_POINT('Ctrl Pts',(-40.2377604171003,3.64393708624685,2.27698460548143));
#25321=CARTESIAN_POINT('Ctrl Pts',(-40.2113020837669,2.32931941133151,4.38081266313611));
#25322=CARTESIAN_POINT('Ctrl Pts',(-40.1848437504336,-0.149957969249583,
4.29423438922274));
#25323=CARTESIAN_POINT('Origin',(-43.8559375004335,-3.93782229046735E-15,
8.32667268468867E-14));
#25324=CARTESIAN_POINT('',(-39.8673437504336,-0.149957969249578,4.29423438922274));
#25325=CARTESIAN_POINT('',(-39.9070312504336,-0.149957969249578,4.29423438922274));
#25326=CARTESIAN_POINT('',(-43.8559375004333,-0.149957969249592,4.2942343892229));
#25327=CARTESIAN_POINT('Ctrl Pts',(-40.2245312504336,-0.149957969249583,
4.29423438922274));
#25328=CARTESIAN_POINT('Ctrl Pts',(-40.1980729171003,-2.62923534983068,
4.20765611530936));
#25329=CARTESIAN_POINT('Ctrl Pts',(-40.1716145837669,-3.79389505549643,
2.01724978374131));
#25330=CARTESIAN_POINT('Ctrl Pts',(-40.1451562504336,-4.95855476116219,
-0.173156547826752));
#25331=CARTESIAN_POINT('Ctrl Pts',(-40.1186979171003,-3.64393708624685,
-2.27698460548143));
#25332=CARTESIAN_POINT('Ctrl Pts',(-40.0922395837669,-2.32931941133151,
-4.38081266313611));
#25333=CARTESIAN_POINT('Ctrl Pts',(-40.0657812504336,0.149957969249583,
-4.29423438922274));
#25334=CARTESIAN_POINT('Ctrl Pts',(-40.0393229171003,2.62923534983068,-4.20765611530936));
#25335=CARTESIAN_POINT('Ctrl Pts',(-40.0128645837669,3.79389505549643,-2.0172497837413));
#25336=CARTESIAN_POINT('Ctrl Pts',(-39.9864062504336,4.95855476116219,0.173156547826753));
#25337=CARTESIAN_POINT('Ctrl Pts',(-39.9599479171003,3.64393708624685,2.27698460548143));
#25338=CARTESIAN_POINT('Ctrl Pts',(-39.9334895837669,2.32931941133151,4.38081266313611));
#25339=CARTESIAN_POINT('Ctrl Pts',(-39.9070312504336,-0.149957969249583,
4.29423438922274));
#25340=CARTESIAN_POINT('Ctrl Pts',(-40.1848437504336,-0.149957969249583,
4.29423438922274));
#25341=CARTESIAN_POINT('Ctrl Pts',(-40.1583854171003,-2.62923534983068,
4.20765611530936));
#25342=CARTESIAN_POINT('Ctrl Pts',(-40.1319270837669,-3.79389505549643,
2.01724978374131));
#25343=CARTESIAN_POINT('Ctrl Pts',(-40.1054687504336,-4.95855476116219,
-0.173156547826752));
#25344=CARTESIAN_POINT('Ctrl Pts',(-40.0790104171003,-3.64393708624685,
-2.27698460548143));
#25345=CARTESIAN_POINT('Ctrl Pts',(-40.0525520837669,-2.32931941133151,
-4.38081266313611));
#25346=CARTESIAN_POINT('Ctrl Pts',(-40.0260937504336,0.149957969249583,
-4.29423438922274));
#25347=CARTESIAN_POINT('Ctrl Pts',(-39.9996354171003,2.62923534983068,-4.20765611530936));
#25348=CARTESIAN_POINT('Ctrl Pts',(-39.9731770837669,3.79389505549644,-2.0172497837413));
#25349=CARTESIAN_POINT('Ctrl Pts',(-39.9467187504336,4.95855476116219,0.173156547826753));
#25350=CARTESIAN_POINT('Ctrl Pts',(-39.9202604171003,3.64393708624685,2.27698460548143));
#25351=CARTESIAN_POINT('Ctrl Pts',(-39.8938020837669,2.32931941133151,4.38081266313611));
#25352=CARTESIAN_POINT('Ctrl Pts',(-39.8673437504336,-0.149957969249583,
4.29423438922274));
#25353=CARTESIAN_POINT('Origin',(-43.8559375004335,-3.93782229046735E-15,
8.32667268468867E-14));
#25354=CARTESIAN_POINT('',(-39.5498437504336,-0.149957969249578,4.29423438922274));
#25355=CARTESIAN_POINT('',(-39.5895312504336,-0.149957969249578,4.29423438922274));
#25356=CARTESIAN_POINT('',(-43.8559375004333,-0.149957969249592,4.2942343892229));
#25357=CARTESIAN_POINT('Ctrl Pts',(-39.9070312504336,-0.149957969249583,
4.29423438922274));
#25358=CARTESIAN_POINT('Ctrl Pts',(-39.8805729171003,-2.62923534983068,
4.20765611530936));
#25359=CARTESIAN_POINT('Ctrl Pts',(-39.8541145837669,-3.79389505549643,
2.01724978374131));
#25360=CARTESIAN_POINT('Ctrl Pts',(-39.8276562504336,-4.95855476116219,
-0.173156547826752));
#25361=CARTESIAN_POINT('Ctrl Pts',(-39.8011979171003,-3.64393708624685,
-2.27698460548143));
#25362=CARTESIAN_POINT('Ctrl Pts',(-39.7747395837669,-2.32931941133151,
-4.38081266313611));
#25363=CARTESIAN_POINT('Ctrl Pts',(-39.7482812504336,0.149957969249583,
-4.29423438922274));
#25364=CARTESIAN_POINT('Ctrl Pts',(-39.7218229171003,2.62923534983068,-4.20765611530936));
#25365=CARTESIAN_POINT('Ctrl Pts',(-39.6953645837669,3.79389505549643,-2.0172497837413));
#25366=CARTESIAN_POINT('Ctrl Pts',(-39.6689062504336,4.95855476116219,0.173156547826753));
#25367=CARTESIAN_POINT('Ctrl Pts',(-39.6424479171003,3.64393708624685,2.27698460548143));
#25368=CARTESIAN_POINT('Ctrl Pts',(-39.6159895837669,2.32931941133151,4.38081266313611));
#25369=CARTESIAN_POINT('Ctrl Pts',(-39.5895312504336,-0.149957969249583,
4.29423438922274));
#25370=CARTESIAN_POINT('Ctrl Pts',(-39.8673437504336,-0.149957969249583,
4.29423438922274));
#25371=CARTESIAN_POINT('Ctrl Pts',(-39.8408854171003,-2.62923534983068,
4.20765611530936));
#25372=CARTESIAN_POINT('Ctrl Pts',(-39.8144270837669,-3.79389505549643,
2.01724978374131));
#25373=CARTESIAN_POINT('Ctrl Pts',(-39.7879687504336,-4.95855476116219,
-0.173156547826752));
#25374=CARTESIAN_POINT('Ctrl Pts',(-39.7615104171003,-3.64393708624685,
-2.27698460548143));
#25375=CARTESIAN_POINT('Ctrl Pts',(-39.7350520837669,-2.32931941133151,
-4.38081266313611));
#25376=CARTESIAN_POINT('Ctrl Pts',(-39.7085937504336,0.149957969249583,
-4.29423438922274));
#25377=CARTESIAN_POINT('Ctrl Pts',(-39.6821354171003,2.62923534983068,-4.20765611530936));
#25378=CARTESIAN_POINT('Ctrl Pts',(-39.6556770837669,3.79389505549644,-2.0172497837413));
#25379=CARTESIAN_POINT('Ctrl Pts',(-39.6292187504336,4.95855476116219,0.173156547826753));
#25380=CARTESIAN_POINT('Ctrl Pts',(-39.6027604171003,3.64393708624685,2.27698460548143));
#25381=CARTESIAN_POINT('Ctrl Pts',(-39.5763020837669,2.32931941133151,4.38081266313611));
#25382=CARTESIAN_POINT('Ctrl Pts',(-39.5498437504336,-0.149957969249583,
4.29423438922274));
#25383=CARTESIAN_POINT('Origin',(-43.8559375004335,-3.93782229046735E-15,
8.32667268468867E-14));
#25384=CARTESIAN_POINT('',(-39.2323437504336,-0.149957969249577,4.29423438922274));
#25385=CARTESIAN_POINT('',(-39.2720312504336,-0.149957969249577,4.29423438922274));
#25386=CARTESIAN_POINT('',(-43.8559375004333,-0.149957969249592,4.2942343892229));
#25387=CARTESIAN_POINT('Ctrl Pts',(-39.5895312504336,-0.149957969249583,
4.29423438922274));
#25388=CARTESIAN_POINT('Ctrl Pts',(-39.5630729171003,-2.62923534983068,
4.20765611530936));
#25389=CARTESIAN_POINT('Ctrl Pts',(-39.5366145837669,-3.79389505549643,
2.01724978374131));
#25390=CARTESIAN_POINT('Ctrl Pts',(-39.5101562504336,-4.95855476116219,
-0.173156547826752));
#25391=CARTESIAN_POINT('Ctrl Pts',(-39.4836979171003,-3.64393708624685,
-2.27698460548143));
#25392=CARTESIAN_POINT('Ctrl Pts',(-39.4572395837669,-2.32931941133151,
-4.38081266313611));
#25393=CARTESIAN_POINT('Ctrl Pts',(-39.4307812504336,0.149957969249583,
-4.29423438922274));
#25394=CARTESIAN_POINT('Ctrl Pts',(-39.4043229171003,2.62923534983068,-4.20765611530936));
#25395=CARTESIAN_POINT('Ctrl Pts',(-39.3778645837669,3.79389505549643,-2.0172497837413));
#25396=CARTESIAN_POINT('Ctrl Pts',(-39.3514062504336,4.95855476116219,0.173156547826753));
#25397=CARTESIAN_POINT('Ctrl Pts',(-39.3249479171003,3.64393708624685,2.27698460548143));
#25398=CARTESIAN_POINT('Ctrl Pts',(-39.2984895837669,2.32931941133151,4.38081266313611));
#25399=CARTESIAN_POINT('Ctrl Pts',(-39.2720312504336,-0.149957969249583,
4.29423438922274));
#25400=CARTESIAN_POINT('Ctrl Pts',(-39.5498437504336,-0.149957969249583,
4.29423438922274));
#25401=CARTESIAN_POINT('Ctrl Pts',(-39.5233854171003,-2.62923534983068,
4.20765611530936));
#25402=CARTESIAN_POINT('Ctrl Pts',(-39.4969270837669,-3.79389505549643,
2.01724978374131));
#25403=CARTESIAN_POINT('Ctrl Pts',(-39.4704687504336,-4.95855476116219,
-0.173156547826752));
#25404=CARTESIAN_POINT('Ctrl Pts',(-39.4440104171003,-3.64393708624685,
-2.27698460548143));
#25405=CARTESIAN_POINT('Ctrl Pts',(-39.4175520837669,-2.32931941133151,
-4.38081266313611));
#25406=CARTESIAN_POINT('Ctrl Pts',(-39.3910937504336,0.149957969249583,
-4.29423438922274));
#25407=CARTESIAN_POINT('Ctrl Pts',(-39.3646354171003,2.62923534983068,-4.20765611530936));
#25408=CARTESIAN_POINT('Ctrl Pts',(-39.3381770837669,3.79389505549644,-2.0172497837413));
#25409=CARTESIAN_POINT('Ctrl Pts',(-39.3117187504336,4.95855476116219,0.173156547826753));
#25410=CARTESIAN_POINT('Ctrl Pts',(-39.2852604171003,3.64393708624685,2.27698460548143));
#25411=CARTESIAN_POINT('Ctrl Pts',(-39.2588020837669,2.32931941133151,4.38081266313611));
#25412=CARTESIAN_POINT('Ctrl Pts',(-39.2323437504336,-0.149957969249583,
4.29423438922274));
#25413=CARTESIAN_POINT('Origin',(-43.8559375004335,-3.93782229046735E-15,
8.32667268468867E-14));
#25414=CARTESIAN_POINT('',(-38.9148437504336,-0.149957969249577,4.29423438922274));
#25415=CARTESIAN_POINT('',(-38.9545312504336,-0.149957969249577,4.29423438922274));
#25416=CARTESIAN_POINT('',(-43.8559375004333,-0.149957969249592,4.2942343892229));
#25417=CARTESIAN_POINT('Ctrl Pts',(-39.2720312504336,-0.149957969249583,
4.29423438922274));
#25418=CARTESIAN_POINT('Ctrl Pts',(-39.2455729171003,-2.62923534983068,
4.20765611530936));
#25419=CARTESIAN_POINT('Ctrl Pts',(-39.2191145837669,-3.79389505549643,
2.01724978374131));
#25420=CARTESIAN_POINT('Ctrl Pts',(-39.1926562504336,-4.95855476116219,
-0.173156547826752));
#25421=CARTESIAN_POINT('Ctrl Pts',(-39.1661979171003,-3.64393708624685,
-2.27698460548143));
#25422=CARTESIAN_POINT('Ctrl Pts',(-39.1397395837669,-2.32931941133151,
-4.38081266313611));
#25423=CARTESIAN_POINT('Ctrl Pts',(-39.1132812504336,0.149957969249583,
-4.29423438922274));
#25424=CARTESIAN_POINT('Ctrl Pts',(-39.0868229171003,2.62923534983068,-4.20765611530936));
#25425=CARTESIAN_POINT('Ctrl Pts',(-39.0603645837669,3.79389505549643,-2.0172497837413));
#25426=CARTESIAN_POINT('Ctrl Pts',(-39.0339062504336,4.95855476116219,0.173156547826753));
#25427=CARTESIAN_POINT('Ctrl Pts',(-39.0074479171003,3.64393708624685,2.27698460548143));
#25428=CARTESIAN_POINT('Ctrl Pts',(-38.9809895837669,2.32931941133151,4.38081266313611));
#25429=CARTESIAN_POINT('Ctrl Pts',(-38.9545312504336,-0.149957969249583,
4.29423438922274));
#25430=CARTESIAN_POINT('Ctrl Pts',(-39.2323437504336,-0.149957969249583,
4.29423438922274));
#25431=CARTESIAN_POINT('Ctrl Pts',(-39.2058854171003,-2.62923534983068,
4.20765611530936));
#25432=CARTESIAN_POINT('Ctrl Pts',(-39.1794270837669,-3.79389505549643,
2.01724978374131));
#25433=CARTESIAN_POINT('Ctrl Pts',(-39.1529687504336,-4.95855476116219,
-0.173156547826752));
#25434=CARTESIAN_POINT('Ctrl Pts',(-39.1265104171003,-3.64393708624685,
-2.27698460548143));
#25435=CARTESIAN_POINT('Ctrl Pts',(-39.1000520837669,-2.32931941133151,
-4.38081266313611));
#25436=CARTESIAN_POINT('Ctrl Pts',(-39.0735937504336,0.149957969249583,
-4.29423438922274));
#25437=CARTESIAN_POINT('Ctrl Pts',(-39.0471354171003,2.62923534983068,-4.20765611530936));
#25438=CARTESIAN_POINT('Ctrl Pts',(-39.0206770837669,3.79389505549644,-2.0172497837413));
#25439=CARTESIAN_POINT('Ctrl Pts',(-38.9942187504336,4.95855476116219,0.173156547826753));
#25440=CARTESIAN_POINT('Ctrl Pts',(-38.9677604171003,3.64393708624685,2.27698460548143));
#25441=CARTESIAN_POINT('Ctrl Pts',(-38.9413020837669,2.32931941133151,4.38081266313611));
#25442=CARTESIAN_POINT('Ctrl Pts',(-38.9148437504336,-0.149957969249583,
4.29423438922274));
#25443=CARTESIAN_POINT('Origin',(-43.8559375004335,-3.93782229046735E-15,
8.32667268468867E-14));
#25444=CARTESIAN_POINT('',(-38.5973437504336,-0.149957969249576,4.29423438922274));
#25445=CARTESIAN_POINT('',(-38.6370312504336,-0.149957969249576,4.29423438922274));
#25446=CARTESIAN_POINT('',(-43.8559375004333,-0.149957969249592,4.2942343892229));
#25447=CARTESIAN_POINT('Ctrl Pts',(-38.9545312504336,-0.149957969249583,
4.29423438922274));
#25448=CARTESIAN_POINT('Ctrl Pts',(-38.9280729171003,-2.62923534983068,
4.20765611530936));
#25449=CARTESIAN_POINT('Ctrl Pts',(-38.9016145837669,-3.79389505549643,
2.01724978374131));
#25450=CARTESIAN_POINT('Ctrl Pts',(-38.8751562504336,-4.95855476116219,
-0.173156547826752));
#25451=CARTESIAN_POINT('Ctrl Pts',(-38.8486979171003,-3.64393708624685,
-2.27698460548143));
#25452=CARTESIAN_POINT('Ctrl Pts',(-38.8222395837669,-2.32931941133151,
-4.38081266313611));
#25453=CARTESIAN_POINT('Ctrl Pts',(-38.7957812504336,0.149957969249583,
-4.29423438922274));
#25454=CARTESIAN_POINT('Ctrl Pts',(-38.7693229171003,2.62923534983068,-4.20765611530936));
#25455=CARTESIAN_POINT('Ctrl Pts',(-38.7428645837669,3.79389505549643,-2.0172497837413));
#25456=CARTESIAN_POINT('Ctrl Pts',(-38.7164062504336,4.95855476116219,0.173156547826753));
#25457=CARTESIAN_POINT('Ctrl Pts',(-38.6899479171003,3.64393708624685,2.27698460548143));
#25458=CARTESIAN_POINT('Ctrl Pts',(-38.6634895837669,2.32931941133151,4.38081266313611));
#25459=CARTESIAN_POINT('Ctrl Pts',(-38.6370312504336,-0.149957969249583,
4.29423438922274));
#25460=CARTESIAN_POINT('Ctrl Pts',(-38.9148437504336,-0.149957969249583,
4.29423438922274));
#25461=CARTESIAN_POINT('Ctrl Pts',(-38.8883854171003,-2.62923534983068,
4.20765611530936));
#25462=CARTESIAN_POINT('Ctrl Pts',(-38.8619270837669,-3.79389505549643,
2.01724978374131));
#25463=CARTESIAN_POINT('Ctrl Pts',(-38.8354687504336,-4.95855476116219,
-0.173156547826752));
#25464=CARTESIAN_POINT('Ctrl Pts',(-38.8090104171003,-3.64393708624685,
-2.27698460548143));
#25465=CARTESIAN_POINT('Ctrl Pts',(-38.7825520837669,-2.32931941133151,
-4.38081266313611));
#25466=CARTESIAN_POINT('Ctrl Pts',(-38.7560937504336,0.149957969249583,
-4.29423438922274));
#25467=CARTESIAN_POINT('Ctrl Pts',(-38.7296354171002,2.62923534983068,-4.20765611530936));
#25468=CARTESIAN_POINT('Ctrl Pts',(-38.7031770837669,3.79389505549644,-2.0172497837413));
#25469=CARTESIAN_POINT('Ctrl Pts',(-38.6767187504336,4.95855476116219,0.173156547826753));
#25470=CARTESIAN_POINT('Ctrl Pts',(-38.6502604171003,3.64393708624685,2.27698460548143));
#25471=CARTESIAN_POINT('Ctrl Pts',(-38.6238020837669,2.32931941133151,4.38081266313611));
#25472=CARTESIAN_POINT('Ctrl Pts',(-38.5973437504336,-0.149957969249583,
4.29423438922274));
#25473=CARTESIAN_POINT('Origin',(-43.8559375004335,-3.93782229046735E-15,
8.32667268468867E-14));
#25474=CARTESIAN_POINT('',(-38.2798437504336,-0.149957969249576,4.29423438922274));
#25475=CARTESIAN_POINT('',(-38.3195312504336,-0.149957969249576,4.29423438922274));
#25476=CARTESIAN_POINT('',(-43.8559375004333,-0.149957969249592,4.2942343892229));
#25477=CARTESIAN_POINT('Ctrl Pts',(-38.6370312504336,-0.149957969249583,
4.29423438922274));
#25478=CARTESIAN_POINT('Ctrl Pts',(-38.6105729171003,-2.62923534983068,
4.20765611530936));
#25479=CARTESIAN_POINT('Ctrl Pts',(-38.5841145837669,-3.79389505549643,
2.01724978374131));
#25480=CARTESIAN_POINT('Ctrl Pts',(-38.5576562504336,-4.95855476116219,
-0.173156547826752));
#25481=CARTESIAN_POINT('Ctrl Pts',(-38.5311979171003,-3.64393708624685,
-2.27698460548143));
#25482=CARTESIAN_POINT('Ctrl Pts',(-38.5047395837669,-2.32931941133151,
-4.38081266313611));
#25483=CARTESIAN_POINT('Ctrl Pts',(-38.4782812504336,0.149957969249583,
-4.29423438922274));
#25484=CARTESIAN_POINT('Ctrl Pts',(-38.4518229171003,2.62923534983068,-4.20765611530936));
#25485=CARTESIAN_POINT('Ctrl Pts',(-38.4253645837669,3.79389505549643,-2.0172497837413));
#25486=CARTESIAN_POINT('Ctrl Pts',(-38.3989062504336,4.95855476116219,0.173156547826753));
#25487=CARTESIAN_POINT('Ctrl Pts',(-38.3724479171003,3.64393708624685,2.27698460548143));
#25488=CARTESIAN_POINT('Ctrl Pts',(-38.3459895837669,2.32931941133151,4.38081266313611));
#25489=CARTESIAN_POINT('Ctrl Pts',(-38.3195312504336,-0.149957969249583,
4.29423438922274));
#25490=CARTESIAN_POINT('Ctrl Pts',(-38.5973437504336,-0.149957969249583,
4.29423438922274));
#25491=CARTESIAN_POINT('Ctrl Pts',(-38.5708854171003,-2.62923534983068,
4.20765611530936));
#25492=CARTESIAN_POINT('Ctrl Pts',(-38.5444270837669,-3.79389505549643,
2.01724978374131));
#25493=CARTESIAN_POINT('Ctrl Pts',(-38.5179687504336,-4.95855476116219,
-0.173156547826752));
#25494=CARTESIAN_POINT('Ctrl Pts',(-38.4915104171003,-3.64393708624685,
-2.27698460548143));
#25495=CARTESIAN_POINT('Ctrl Pts',(-38.4650520837669,-2.32931941133151,
-4.38081266313611));
#25496=CARTESIAN_POINT('Ctrl Pts',(-38.4385937504336,0.149957969249583,
-4.29423438922274));
#25497=CARTESIAN_POINT('Ctrl Pts',(-38.4121354171003,2.62923534983068,-4.20765611530936));
#25498=CARTESIAN_POINT('Ctrl Pts',(-38.3856770837669,3.79389505549644,-2.0172497837413));
#25499=CARTESIAN_POINT('Ctrl Pts',(-38.3592187504336,4.95855476116219,0.173156547826753));
#25500=CARTESIAN_POINT('Ctrl Pts',(-38.3327604171003,3.64393708624685,2.27698460548143));
#25501=CARTESIAN_POINT('Ctrl Pts',(-38.3063020837669,2.32931941133151,4.38081266313611));
#25502=CARTESIAN_POINT('Ctrl Pts',(-38.2798437504336,-0.149957969249583,
4.29423438922274));
#25503=CARTESIAN_POINT('Origin',(-43.8559375004335,-3.93782229046735E-15,
8.32667268468867E-14));
#25504=CARTESIAN_POINT('',(-37.9623437504336,-0.149957969249575,4.29423438922274));
#25505=CARTESIAN_POINT('',(-38.0020312504336,-0.149957969249575,4.29423438922274));
#25506=CARTESIAN_POINT('',(-43.8559375004333,-0.149957969249592,4.2942343892229));
#25507=CARTESIAN_POINT('Ctrl Pts',(-38.3195312504336,-0.149957969249583,
4.29423438922274));
#25508=CARTESIAN_POINT('Ctrl Pts',(-38.2930729171002,-2.62923534983068,
4.20765611530936));
#25509=CARTESIAN_POINT('Ctrl Pts',(-38.2666145837669,-3.79389505549643,
2.01724978374131));
#25510=CARTESIAN_POINT('Ctrl Pts',(-38.2401562504336,-4.95855476116219,
-0.173156547826752));
#25511=CARTESIAN_POINT('Ctrl Pts',(-38.2136979171003,-3.64393708624685,
-2.27698460548143));
#25512=CARTESIAN_POINT('Ctrl Pts',(-38.1872395837669,-2.32931941133151,
-4.38081266313611));
#25513=CARTESIAN_POINT('Ctrl Pts',(-38.1607812504336,0.149957969249583,
-4.29423438922274));
#25514=CARTESIAN_POINT('Ctrl Pts',(-38.1343229171002,2.62923534983068,-4.20765611530936));
#25515=CARTESIAN_POINT('Ctrl Pts',(-38.1078645837669,3.79389505549643,-2.0172497837413));
#25516=CARTESIAN_POINT('Ctrl Pts',(-38.0814062504336,4.95855476116219,0.173156547826753));
#25517=CARTESIAN_POINT('Ctrl Pts',(-38.0549479171003,3.64393708624685,2.27698460548143));
#25518=CARTESIAN_POINT('Ctrl Pts',(-38.0284895837669,2.32931941133151,4.38081266313611));
#25519=CARTESIAN_POINT('Ctrl Pts',(-38.0020312504336,-0.149957969249583,
4.29423438922274));
#25520=CARTESIAN_POINT('Ctrl Pts',(-38.2798437504336,-0.149957969249583,
4.29423438922274));
#25521=CARTESIAN_POINT('Ctrl Pts',(-38.2533854171003,-2.62923534983068,
4.20765611530936));
#25522=CARTESIAN_POINT('Ctrl Pts',(-38.2269270837669,-3.79389505549643,
2.01724978374131));
#25523=CARTESIAN_POINT('Ctrl Pts',(-38.2004687504336,-4.95855476116219,
-0.173156547826752));
#25524=CARTESIAN_POINT('Ctrl Pts',(-38.1740104171002,-3.64393708624685,
-2.27698460548143));
#25525=CARTESIAN_POINT('Ctrl Pts',(-38.1475520837669,-2.32931941133151,
-4.38081266313611));
#25526=CARTESIAN_POINT('Ctrl Pts',(-38.1210937504336,0.149957969249583,
-4.29423438922274));
#25527=CARTESIAN_POINT('Ctrl Pts',(-38.0946354171003,2.62923534983068,-4.20765611530936));
#25528=CARTESIAN_POINT('Ctrl Pts',(-38.0681770837669,3.79389505549644,-2.0172497837413));
#25529=CARTESIAN_POINT('Ctrl Pts',(-38.0417187504336,4.95855476116219,0.173156547826753));
#25530=CARTESIAN_POINT('Ctrl Pts',(-38.0152604171003,3.64393708624685,2.27698460548143));
#25531=CARTESIAN_POINT('Ctrl Pts',(-37.9888020837669,2.32931941133151,4.38081266313611));
#25532=CARTESIAN_POINT('Ctrl Pts',(-37.9623437504336,-0.149957969249583,
4.29423438922274));
#25533=CARTESIAN_POINT('Origin',(-43.8559375004335,-3.93782229046735E-15,
8.32667268468867E-14));
#25534=CARTESIAN_POINT('',(-37.6448437504336,-0.149957969249575,4.29423438922274));
#25535=CARTESIAN_POINT('',(-37.6845312504336,-0.149957969249575,4.29423438922274));
#25536=CARTESIAN_POINT('',(-43.8559375004333,-0.149957969249592,4.2942343892229));
#25537=CARTESIAN_POINT('Ctrl Pts',(-38.0020312504336,-0.149957969249583,
4.29423438922274));
#25538=CARTESIAN_POINT('Ctrl Pts',(-37.9755729171003,-2.62923534983068,
4.20765611530936));
#25539=CARTESIAN_POINT('Ctrl Pts',(-37.9491145837669,-3.79389505549643,
2.01724978374131));
#25540=CARTESIAN_POINT('Ctrl Pts',(-37.9226562504336,-4.95855476116219,
-0.173156547826752));
#25541=CARTESIAN_POINT('Ctrl Pts',(-37.8961979171003,-3.64393708624685,
-2.27698460548143));
#25542=CARTESIAN_POINT('Ctrl Pts',(-37.8697395837669,-2.32931941133151,
-4.38081266313611));
#25543=CARTESIAN_POINT('Ctrl Pts',(-37.8432812504336,0.149957969249583,
-4.29423438922274));
#25544=CARTESIAN_POINT('Ctrl Pts',(-37.8168229171003,2.62923534983068,-4.20765611530936));
#25545=CARTESIAN_POINT('Ctrl Pts',(-37.7903645837669,3.79389505549643,-2.0172497837413));
#25546=CARTESIAN_POINT('Ctrl Pts',(-37.7639062504336,4.95855476116219,0.173156547826753));
#25547=CARTESIAN_POINT('Ctrl Pts',(-37.7374479171003,3.64393708624685,2.27698460548143));
#25548=CARTESIAN_POINT('Ctrl Pts',(-37.7109895837669,2.32931941133151,4.38081266313611));
#25549=CARTESIAN_POINT('Ctrl Pts',(-37.6845312504336,-0.149957969249583,
4.29423438922274));
#25550=CARTESIAN_POINT('Ctrl Pts',(-37.9623437504336,-0.149957969249583,
4.29423438922274));
#25551=CARTESIAN_POINT('Ctrl Pts',(-37.9358854171002,-2.62923534983068,
4.20765611530936));
#25552=CARTESIAN_POINT('Ctrl Pts',(-37.9094270837669,-3.79389505549643,
2.01724978374131));
#25553=CARTESIAN_POINT('Ctrl Pts',(-37.8829687504336,-4.95855476116219,
-0.173156547826752));
#25554=CARTESIAN_POINT('Ctrl Pts',(-37.8565104171003,-3.64393708624685,
-2.27698460548143));
#25555=CARTESIAN_POINT('Ctrl Pts',(-37.8300520837669,-2.32931941133151,
-4.38081266313611));
#25556=CARTESIAN_POINT('Ctrl Pts',(-37.8035937504336,0.149957969249583,
-4.29423438922274));
#25557=CARTESIAN_POINT('Ctrl Pts',(-37.7771354171003,2.62923534983068,-4.20765611530936));
#25558=CARTESIAN_POINT('Ctrl Pts',(-37.7506770837669,3.79389505549644,-2.0172497837413));
#25559=CARTESIAN_POINT('Ctrl Pts',(-37.7242187504336,4.95855476116219,0.173156547826753));
#25560=CARTESIAN_POINT('Ctrl Pts',(-37.6977604171003,3.64393708624685,2.27698460548143));
#25561=CARTESIAN_POINT('Ctrl Pts',(-37.6713020837669,2.32931941133151,4.38081266313611));
#25562=CARTESIAN_POINT('Ctrl Pts',(-37.6448437504336,-0.149957969249583,
4.29423438922274));
#25563=CARTESIAN_POINT('Origin',(-43.8559375004335,-3.93782229046735E-15,
8.32667268468867E-14));
#25564=CARTESIAN_POINT('',(-37.3273437504336,-0.149957969249574,4.29423438922274));
#25565=CARTESIAN_POINT('',(-37.3670312504336,-0.149957969249574,4.29423438922274));
#25566=CARTESIAN_POINT('',(-43.8559375004333,-0.149957969249592,4.2942343892229));
#25567=CARTESIAN_POINT('Ctrl Pts',(-37.6845312504336,-0.149957969249583,
4.29423438922274));
#25568=CARTESIAN_POINT('Ctrl Pts',(-37.6580729171003,-2.62923534983068,
4.20765611530936));
#25569=CARTESIAN_POINT('Ctrl Pts',(-37.6316145837669,-3.79389505549643,
2.01724978374131));
#25570=CARTESIAN_POINT('Ctrl Pts',(-37.6051562504336,-4.95855476116219,
-0.173156547826752));
#25571=CARTESIAN_POINT('Ctrl Pts',(-37.5786979171003,-3.64393708624685,
-2.27698460548143));
#25572=CARTESIAN_POINT('Ctrl Pts',(-37.5522395837669,-2.32931941133151,
-4.38081266313611));
#25573=CARTESIAN_POINT('Ctrl Pts',(-37.5257812504336,0.149957969249583,
-4.29423438922274));
#25574=CARTESIAN_POINT('Ctrl Pts',(-37.4993229171003,2.62923534983068,-4.20765611530936));
#25575=CARTESIAN_POINT('Ctrl Pts',(-37.4728645837669,3.79389505549643,-2.0172497837413));
#25576=CARTESIAN_POINT('Ctrl Pts',(-37.4464062504336,4.95855476116219,0.173156547826753));
#25577=CARTESIAN_POINT('Ctrl Pts',(-37.4199479171003,3.64393708624685,2.27698460548143));
#25578=CARTESIAN_POINT('Ctrl Pts',(-37.3934895837669,2.32931941133151,4.38081266313611));
#25579=CARTESIAN_POINT('Ctrl Pts',(-37.3670312504336,-0.149957969249583,
4.29423438922274));
#25580=CARTESIAN_POINT('Ctrl Pts',(-37.6448437504336,-0.149957969249583,
4.29423438922274));
#25581=CARTESIAN_POINT('Ctrl Pts',(-37.6183854171003,-2.62923534983068,
4.20765611530936));
#25582=CARTESIAN_POINT('Ctrl Pts',(-37.5919270837669,-3.79389505549643,
2.01724978374131));
#25583=CARTESIAN_POINT('Ctrl Pts',(-37.5654687504336,-4.95855476116219,
-0.173156547826752));
#25584=CARTESIAN_POINT('Ctrl Pts',(-37.5390104171003,-3.64393708624685,
-2.27698460548143));
#25585=CARTESIAN_POINT('Ctrl Pts',(-37.5125520837669,-2.32931941133151,
-4.38081266313611));
#25586=CARTESIAN_POINT('Ctrl Pts',(-37.4860937504336,0.149957969249583,
-4.29423438922274));
#25587=CARTESIAN_POINT('Ctrl Pts',(-37.4596354171003,2.62923534983068,-4.20765611530936));
#25588=CARTESIAN_POINT('Ctrl Pts',(-37.4331770837669,3.79389505549644,-2.0172497837413));
#25589=CARTESIAN_POINT('Ctrl Pts',(-37.4067187504336,4.95855476116219,0.173156547826753));
#25590=CARTESIAN_POINT('Ctrl Pts',(-37.3802604171003,3.64393708624685,2.27698460548143));
#25591=CARTESIAN_POINT('Ctrl Pts',(-37.3538020837669,2.32931941133151,4.38081266313611));
#25592=CARTESIAN_POINT('Ctrl Pts',(-37.3273437504336,-0.149957969249583,
4.29423438922274));
#25593=CARTESIAN_POINT('Origin',(-43.8559375004335,-3.93782229046735E-15,
8.32667268468867E-14));
#25594=CARTESIAN_POINT('',(-37.0098437504336,-0.149957969249574,4.29423438922274));
#25595=CARTESIAN_POINT('',(-37.0495312504336,-0.149957969249574,4.29423438922274));
#25596=CARTESIAN_POINT('',(-43.8559375004333,-0.149957969249592,4.2942343892229));
#25597=CARTESIAN_POINT('Ctrl Pts',(-37.3670312504336,-0.149957969249583,
4.29423438922274));
#25598=CARTESIAN_POINT('Ctrl Pts',(-37.3405729171003,-2.62923534983068,
4.20765611530936));
#25599=CARTESIAN_POINT('Ctrl Pts',(-37.3141145837669,-3.79389505549643,
2.01724978374131));
#25600=CARTESIAN_POINT('Ctrl Pts',(-37.2876562504336,-4.95855476116219,
-0.173156547826752));
#25601=CARTESIAN_POINT('Ctrl Pts',(-37.2611979171003,-3.64393708624685,
-2.27698460548143));
#25602=CARTESIAN_POINT('Ctrl Pts',(-37.2347395837669,-2.32931941133151,
-4.38081266313611));
#25603=CARTESIAN_POINT('Ctrl Pts',(-37.2082812504336,0.149957969249583,
-4.29423438922274));
#25604=CARTESIAN_POINT('Ctrl Pts',(-37.1818229171003,2.62923534983068,-4.20765611530936));
#25605=CARTESIAN_POINT('Ctrl Pts',(-37.1553645837669,3.79389505549643,-2.0172497837413));
#25606=CARTESIAN_POINT('Ctrl Pts',(-37.1289062504336,4.95855476116219,0.173156547826753));
#25607=CARTESIAN_POINT('Ctrl Pts',(-37.1024479171003,3.64393708624685,2.27698460548143));
#25608=CARTESIAN_POINT('Ctrl Pts',(-37.0759895837669,2.32931941133151,4.38081266313611));
#25609=CARTESIAN_POINT('Ctrl Pts',(-37.0495312504336,-0.149957969249583,
4.29423438922274));
#25610=CARTESIAN_POINT('Ctrl Pts',(-37.3273437504336,-0.149957969249583,
4.29423438922274));
#25611=CARTESIAN_POINT('Ctrl Pts',(-37.3008854171003,-2.62923534983068,
4.20765611530936));
#25612=CARTESIAN_POINT('Ctrl Pts',(-37.2744270837669,-3.79389505549643,
2.01724978374131));
#25613=CARTESIAN_POINT('Ctrl Pts',(-37.2479687504336,-4.95855476116219,
-0.173156547826752));
#25614=CARTESIAN_POINT('Ctrl Pts',(-37.2215104171003,-3.64393708624685,
-2.27698460548143));
#25615=CARTESIAN_POINT('Ctrl Pts',(-37.1950520837669,-2.32931941133151,
-4.38081266313611));
#25616=CARTESIAN_POINT('Ctrl Pts',(-37.1685937504336,0.149957969249583,
-4.29423438922274));
#25617=CARTESIAN_POINT('Ctrl Pts',(-37.1421354171003,2.62923534983068,-4.20765611530936));
#25618=CARTESIAN_POINT('Ctrl Pts',(-37.1156770837669,3.79389505549644,-2.0172497837413));
#25619=CARTESIAN_POINT('Ctrl Pts',(-37.0892187504336,4.95855476116219,0.173156547826753));
#25620=CARTESIAN_POINT('Ctrl Pts',(-37.0627604171003,3.64393708624685,2.27698460548143));
#25621=CARTESIAN_POINT('Ctrl Pts',(-37.0363020837669,2.32931941133151,4.38081266313611));
#25622=CARTESIAN_POINT('Ctrl Pts',(-37.0098437504336,-0.149957969249583,
4.29423438922274));
#25623=CARTESIAN_POINT('Origin',(-43.8559375004335,-3.93782229046735E-15,
8.32667268468867E-14));
#25624=CARTESIAN_POINT('',(-36.6923437504336,-0.149957969249573,4.29423438922274));
#25625=CARTESIAN_POINT('',(-36.7320312504336,-0.149957969249573,4.29423438922274));
#25626=CARTESIAN_POINT('',(-43.8559375004333,-0.149957969249592,4.2942343892229));
#25627=CARTESIAN_POINT('Ctrl Pts',(-37.0495312504336,-0.149957969249583,
4.29423438922274));
#25628=CARTESIAN_POINT('Ctrl Pts',(-37.0230729171003,-2.62923534983068,
4.20765611530936));
#25629=CARTESIAN_POINT('Ctrl Pts',(-36.9966145837669,-3.79389505549643,
2.01724978374131));
#25630=CARTESIAN_POINT('Ctrl Pts',(-36.9701562504336,-4.95855476116219,
-0.173156547826752));
#25631=CARTESIAN_POINT('Ctrl Pts',(-36.9436979171003,-3.64393708624685,
-2.27698460548143));
#25632=CARTESIAN_POINT('Ctrl Pts',(-36.9172395837669,-2.32931941133151,
-4.38081266313611));
#25633=CARTESIAN_POINT('Ctrl Pts',(-36.8907812504336,0.149957969249583,
-4.29423438922274));
#25634=CARTESIAN_POINT('Ctrl Pts',(-36.8643229171003,2.62923534983068,-4.20765611530936));
#25635=CARTESIAN_POINT('Ctrl Pts',(-36.8378645837669,3.79389505549643,-2.0172497837413));
#25636=CARTESIAN_POINT('Ctrl Pts',(-36.8114062504336,4.95855476116219,0.173156547826753));
#25637=CARTESIAN_POINT('Ctrl Pts',(-36.7849479171003,3.64393708624685,2.27698460548143));
#25638=CARTESIAN_POINT('Ctrl Pts',(-36.7584895837669,2.32931941133151,4.38081266313611));
#25639=CARTESIAN_POINT('Ctrl Pts',(-36.7320312504336,-0.149957969249583,
4.29423438922274));
#25640=CARTESIAN_POINT('Ctrl Pts',(-37.0098437504336,-0.149957969249583,
4.29423438922274));
#25641=CARTESIAN_POINT('Ctrl Pts',(-36.9833854171003,-2.62923534983068,
4.20765611530936));
#25642=CARTESIAN_POINT('Ctrl Pts',(-36.9569270837669,-3.79389505549643,
2.01724978374131));
#25643=CARTESIAN_POINT('Ctrl Pts',(-36.9304687504336,-4.95855476116219,
-0.173156547826752));
#25644=CARTESIAN_POINT('Ctrl Pts',(-36.9040104171003,-3.64393708624685,
-2.27698460548143));
#25645=CARTESIAN_POINT('Ctrl Pts',(-36.8775520837669,-2.32931941133151,
-4.38081266313611));
#25646=CARTESIAN_POINT('Ctrl Pts',(-36.8510937504336,0.149957969249583,
-4.29423438922274));
#25647=CARTESIAN_POINT('Ctrl Pts',(-36.8246354171003,2.62923534983068,-4.20765611530936));
#25648=CARTESIAN_POINT('Ctrl Pts',(-36.7981770837669,3.79389505549644,-2.0172497837413));
#25649=CARTESIAN_POINT('Ctrl Pts',(-36.7717187504336,4.95855476116219,0.173156547826753));
#25650=CARTESIAN_POINT('Ctrl Pts',(-36.7452604171003,3.64393708624685,2.27698460548143));
#25651=CARTESIAN_POINT('Ctrl Pts',(-36.7188020837669,2.32931941133151,4.38081266313611));
#25652=CARTESIAN_POINT('Ctrl Pts',(-36.6923437504336,-0.149957969249583,
4.29423438922274));
#25653=CARTESIAN_POINT('Origin',(-43.8559375004335,-3.93782229046735E-15,
8.32667268468867E-14));
#25654=CARTESIAN_POINT('',(-36.3748437504336,-0.149957969249573,4.29423438922274));
#25655=CARTESIAN_POINT('',(-36.4145312504336,-0.149957969249573,4.29423438922274));
#25656=CARTESIAN_POINT('',(-43.8559375004333,-0.149957969249592,4.2942343892229));
#25657=CARTESIAN_POINT('Ctrl Pts',(-36.7320312504336,-0.149957969249583,
4.29423438922274));
#25658=CARTESIAN_POINT('Ctrl Pts',(-36.7055729171003,-2.62923534983068,
4.20765611530936));
#25659=CARTESIAN_POINT('Ctrl Pts',(-36.6791145837669,-3.79389505549643,
2.01724978374131));
#25660=CARTESIAN_POINT('Ctrl Pts',(-36.6526562504336,-4.95855476116219,
-0.173156547826752));
#25661=CARTESIAN_POINT('Ctrl Pts',(-36.6261979171003,-3.64393708624685,
-2.27698460548143));
#25662=CARTESIAN_POINT('Ctrl Pts',(-36.5997395837669,-2.32931941133151,
-4.38081266313611));
#25663=CARTESIAN_POINT('Ctrl Pts',(-36.5732812504336,0.149957969249583,
-4.29423438922274));
#25664=CARTESIAN_POINT('Ctrl Pts',(-36.5468229171003,2.62923534983068,-4.20765611530936));
#25665=CARTESIAN_POINT('Ctrl Pts',(-36.5203645837669,3.79389505549643,-2.0172497837413));
#25666=CARTESIAN_POINT('Ctrl Pts',(-36.4939062504336,4.95855476116219,0.173156547826753));
#25667=CARTESIAN_POINT('Ctrl Pts',(-36.4674479171003,3.64393708624685,2.27698460548143));
#25668=CARTESIAN_POINT('Ctrl Pts',(-36.4409895837669,2.32931941133151,4.38081266313611));
#25669=CARTESIAN_POINT('Ctrl Pts',(-36.4145312504336,-0.149957969249583,
4.29423438922274));
#25670=CARTESIAN_POINT('Ctrl Pts',(-36.6923437504336,-0.149957969249583,
4.29423438922274));
#25671=CARTESIAN_POINT('Ctrl Pts',(-36.6658854171003,-2.62923534983068,
4.20765611530936));
#25672=CARTESIAN_POINT('Ctrl Pts',(-36.6394270837669,-3.79389505549643,
2.01724978374131));
#25673=CARTESIAN_POINT('Ctrl Pts',(-36.6129687504336,-4.95855476116219,
-0.173156547826752));
#25674=CARTESIAN_POINT('Ctrl Pts',(-36.5865104171002,-3.64393708624685,
-2.27698460548143));
#25675=CARTESIAN_POINT('Ctrl Pts',(-36.5600520837669,-2.32931941133151,
-4.38081266313611));
#25676=CARTESIAN_POINT('Ctrl Pts',(-36.5335937504336,0.149957969249583,
-4.29423438922274));
#25677=CARTESIAN_POINT('Ctrl Pts',(-36.5071354171003,2.62923534983068,-4.20765611530936));
#25678=CARTESIAN_POINT('Ctrl Pts',(-36.4806770837669,3.79389505549644,-2.0172497837413));
#25679=CARTESIAN_POINT('Ctrl Pts',(-36.4542187504336,4.95855476116219,0.173156547826753));
#25680=CARTESIAN_POINT('Ctrl Pts',(-36.4277604171003,3.64393708624685,2.27698460548143));
#25681=CARTESIAN_POINT('Ctrl Pts',(-36.4013020837669,2.32931941133151,4.38081266313611));
#25682=CARTESIAN_POINT('Ctrl Pts',(-36.3748437504336,-0.149957969249583,
4.29423438922274));
#25683=CARTESIAN_POINT('Origin',(-43.8559375004335,-3.93782229046735E-15,
8.32667268468867E-14));
#25684=CARTESIAN_POINT('',(-36.0573437504336,-0.149957969249572,4.29423438922274));
#25685=CARTESIAN_POINT('',(-36.0970312504336,-0.149957969249572,4.29423438922274));
#25686=CARTESIAN_POINT('',(-43.8559375004333,-0.149957969249592,4.2942343892229));
#25687=CARTESIAN_POINT('',(-36.,-3.96679264203451,1.65151219106173));
#25688=CARTESIAN_POINT('Ctrl Pts',(-36.0573437504336,-0.149957969249583,
4.29423438922274));
#25689=CARTESIAN_POINT('Ctrl Pts',(-36.0308854171003,-2.62923534983068,
4.20765611530936));
#25690=CARTESIAN_POINT('Ctrl Pts',(-36.0044270837669,-3.79389505549643,
2.01724978374131));
#25691=CARTESIAN_POINT('Ctrl Pts',(-36.0022673883541,-3.88896189860283,
1.83845505593417));
#25692=CARTESIAN_POINT('Ctrl Pts',(-36.,-3.96679264203451,1.65151219106173));
#25693=CARTESIAN_POINT('',(-36.,-3.99810942017506,-1.57418469260506));
#25694=CARTESIAN_POINT('Origin',(-35.9999999999998,1.55431223447522E-14,
3.88578058618805E-15));
#25695=CARTESIAN_POINT('Ctrl Pts',(-36.0970312504336,-0.149957969249583,
4.29423438922274));
#25696=CARTESIAN_POINT('Ctrl Pts',(-36.0705729171003,-2.62923534983068,
4.20765611530936));
#25697=CARTESIAN_POINT('Ctrl Pts',(-36.0441145837669,-3.79389505549643,
2.01724978374131));
#25698=CARTESIAN_POINT('Ctrl Pts',(-36.0229922517456,-4.72367126947973,
0.268595051253399));
#25699=CARTESIAN_POINT('Ctrl Pts',(-36.,-3.99810942017506,-1.57418469260506));
#25700=CARTESIAN_POINT('Origin',(-44.,0.,0.));
#25701=CARTESIAN_POINT('',(-43.6591154631359,-2.96734935548908E-14,-4.12499999999999));
#25702=CARTESIAN_POINT('',(-43.975,-5.05166804648283E-16,-4.125));
#25703=CARTESIAN_POINT('',(-44.,-5.05166804648282E-16,-4.12499999999999));
#25704=CARTESIAN_POINT('',(-43.975,0.143960423897816,-4.12248716145376));
#25705=CARTESIAN_POINT('Origin',(-43.975,0.,0.));
#25706=CARTESIAN_POINT('Ctrl Pts',(-43.975,0.143960423897817,-4.12248716145376));
#25707=CARTESIAN_POINT('Ctrl Pts',(-43.97183047655,0.42908205717337,-4.11253049462104));
#25708=CARTESIAN_POINT('Ctrl Pts',(-43.9684796639578,0.712401235868628,
-4.07302110630467));
#25709=CARTESIAN_POINT('Ctrl Pts',(-43.9614044274671,1.27578409938326,-3.93383307652861));
#25710=CARTESIAN_POINT('Ctrl Pts',(-43.9576915174157,1.5537851359483,-3.83254723024597));
#25711=CARTESIAN_POINT('Ctrl Pts',(-43.9469595135523,2.30860116593424,-3.46179456351789));
#25712=CARTESIAN_POINT('Ctrl Pts',(-43.9399198814115,2.74599034187203,-3.12621199461402));
#25713=CARTESIAN_POINT('Ctrl Pts',(-43.926701044641,3.45463635345407,-2.31575107321194));
#25714=CARTESIAN_POINT('Ctrl Pts',(-43.9210432976051,3.72358343109977,-1.85260371719902));
#25715=CARTESIAN_POINT('Ctrl Pts',(-43.9083349580575,4.07146299165201,-0.849201559422838));
#25716=CARTESIAN_POINT('Ctrl Pts',(-43.9015615552565,4.1468869566712,-0.318240438634118));
#25717=CARTESIAN_POINT('Ctrl Pts',(-43.8877402455277,4.09140360287742,0.757887952165817));
#25718=CARTESIAN_POINT('Ctrl Pts',(-43.8808265278912,3.95520891889208,1.29240378216373));
#25719=CARTESIAN_POINT('Ctrl Pts',(-43.8682704646471,3.49291086949633,2.2556363213478));
#25720=CARTESIAN_POINT('Ctrl Pts',(-43.862586857156,3.17960346670654,2.67926241239808));
#25721=CARTESIAN_POINT('Ctrl Pts',(-43.8494371722728,2.40047974876652,3.39736504387608));
#25722=CARTESIAN_POINT('Ctrl Pts',(-43.8424910107108,1.93795931290139,3.68085640262762));
#25723=CARTESIAN_POINT('Ctrl Pts',(-43.8287169242127,0.922157190792934,
4.05750959759151));
#25724=CARTESIAN_POINT('Ctrl Pts',(-43.8220687964696,0.37758007752296,4.1438107711559));
#25725=CARTESIAN_POINT('Ctrl Pts',(-43.8101464836354,-0.691107827936443,
4.1002599887138));
#25726=CARTESIAN_POINT('Ctrl Pts',(-43.8037303692132,-1.20543875210143,
3.97953133305015));
#25727=CARTESIAN_POINT('Ctrl Pts',(-43.7901672681873,-2.17995049430338,
3.54390218815809));
#25728=CARTESIAN_POINT('Ctrl Pts',(-43.7831344521376,-2.62771130704635,
3.22592037575174));
#25729=CARTESIAN_POINT('Ctrl Pts',(-43.7697429236182,-3.36811592255533,
2.44088035666596));
#25730=CARTESIAN_POINT('Ctrl Pts',(-43.7639441873864,-3.65607854757604,
1.98373089093437));
#25731=CARTESIAN_POINT('Ctrl Pts',(-43.7513792883756,-4.039229064548,0.990285445042111));
#25732=CARTESIAN_POINT('Ctrl Pts',(-43.7446755248126,-4.13287097726785,
0.464120018982602));
#25733=CARTESIAN_POINT('Ctrl Pts',(-43.7308201405905,-4.11575799333123,
-0.616006114386392));
#25734=CARTESIAN_POINT('Ctrl Pts',(-43.7238005094659,-3.99684332011726,
-1.15938665648937));
#25735=CARTESIAN_POINT('Ctrl Pts',(-43.7110028898235,-3.56364185673055,
-2.14247673551862));
#25736=CARTESIAN_POINT('Ctrl Pts',(-43.7053995962841,-3.2632209128958,-2.57704110067067));
#25737=CARTESIAN_POINT('Ctrl Pts',(-43.6923686904007,-2.50729211492382,
-3.31904453736047));
#25738=CARTESIAN_POINT('Ctrl Pts',(-43.6854620394096,-2.05555241197391,
-3.61625102775665));
#25739=CARTESIAN_POINT('Ctrl Pts',(-43.6717983243574,-1.06445018626301,
-4.02103149758079));
#25740=CARTESIAN_POINT('Ctrl Pts',(-43.665171886146,-0.534703156090073,
-4.12499999999998));
#25741=CARTESIAN_POINT('Ctrl Pts',(-43.6591154631359,-5.91193760612896E-14,
-4.12499999999999));
#25742=CARTESIAN_POINT('Origin',(-44.,0.,0.));
#25743=CARTESIAN_POINT('',(-43.3416154631359,-7.91110547264604E-17,-4.12499999999999));
#25744=CARTESIAN_POINT('',(-43.4209904640031,1.3975723041988E-15,-4.12499999999999));
#25745=CARTESIAN_POINT('',(-44.,-5.05166804648282E-16,-4.12499999999999));
#25746=CARTESIAN_POINT('',(-43.7368750008672,0.143960423897816,-4.12248716145376));
#25747=CARTESIAN_POINT('Ctrl Pts',(-43.4209904640031,2.15305958091061E-15,
-4.12499999999999));
#25748=CARTESIAN_POINT('Ctrl Pts',(-43.4217841869206,-0.0700753808536829,
-4.12499999999999));
#25749=CARTESIAN_POINT('Ctrl Pts',(-43.4225893565914,-0.140211920515319,
-4.12321436266605));
#25750=CARTESIAN_POINT('Ctrl Pts',(-43.4297513900091,-0.755813543173842,
-4.09178269975688));
#25751=CARTESIAN_POINT('Ctrl Pts',(-43.4366245347121,-1.29035673936744,
-3.9558704357677));
#25752=CARTESIAN_POINT('Ctrl Pts',(-43.4504515973494,-2.26318535354331,
-3.48959947740471));
#25753=CARTESIAN_POINT('Ctrl Pts',(-43.4572693723953,-2.69439006697297,
-3.16852957206712));
#25754=CARTESIAN_POINT('Ctrl Pts',(-43.4700762553883,-3.40773676952694,
-2.38363843237575));
#25755=CARTESIAN_POINT('Ctrl Pts',(-43.4756773460284,-3.68454947045869,
-1.92834064584949));
#25756=CARTESIAN_POINT('Ctrl Pts',(-43.4887723270657,-4.0581868735389,-0.919976274451078));
#25757=CARTESIAN_POINT('Ctrl Pts',(-43.4958111522624,-4.14432035210699,
-0.373953844976087));
#25758=CARTESIAN_POINT('Ctrl Pts',(-43.5095479626073,-4.09929622803357,
0.699093369405077));
#25759=CARTESIAN_POINT('Ctrl Pts',(-43.5161225895255,-3.97666071527261,
1.21619858092205));
#25760=CARTESIAN_POINT('Ctrl Pts',(-43.5284456204229,-3.53610661035621,
2.19278282575447));
#25761=CARTESIAN_POINT('Ctrl Pts',(-43.5346273063288,-3.2159594271141,2.64006840117702));
#25762=CARTESIAN_POINT('Ctrl Pts',(-43.548289156452,-2.42346414910966,3.38151107493627));
#25763=CARTESIAN_POINT('Ctrl Pts',(-43.5552899990205,-1.95998718715836,
3.66963839353035));
#25764=CARTESIAN_POINT('Ctrl Pts',(-43.568648828934,-0.966014596552634,
4.04407476096784));
#25765=CARTESIAN_POINT('Ctrl Pts',(-43.5746204731358,-0.447397812110882,
4.13370889184485));
#25766=CARTESIAN_POINT('Ctrl Pts',(-43.5868280322708,0.620166584767352,
4.11451824490259));
#25767=CARTESIAN_POINT('Ctrl Pts',(-43.5936410341835,1.15884306831965,3.99636589021096));
#25768=CARTESIAN_POINT('Ctrl Pts',(-43.6074622740015,2.1480569720669,3.56187802156145));
#25769=CARTESIAN_POINT('Ctrl Pts',(-43.6143324413542,2.59089238020419,3.25398286351057));
#25770=CARTESIAN_POINT('Ctrl Pts',(-43.6272659039809,3.32812620798997,2.49299913232278));
#25771=CARTESIAN_POINT('Ctrl Pts',(-43.6328450895579,3.61818537549182,2.04943959497307));
#25772=CARTESIAN_POINT('Ctrl Pts',(-43.6457747740852,4.0254168025233,1.05514152540184));
#25773=CARTESIAN_POINT('Ctrl Pts',(-43.6528057791958,4.12999005714525,0.510372995931821));
#25774=CARTESIAN_POINT('Ctrl Pts',(-43.6666147684555,4.11984170736092,-0.567086304521003));
#25775=CARTESIAN_POINT('Ctrl Pts',(-43.6732645340858,4.01344136503595,-1.08948541134691));
#25776=CARTESIAN_POINT('Ctrl Pts',(-43.6857251858634,3.60524496755625,-2.07567416616227));
#25777=CARTESIAN_POINT('Ctrl Pts',(-43.6916675575682,3.30343334572731,-2.52854662486236));
#25778=CARTESIAN_POINT('Ctrl Pts',(-43.7049785336112,2.55166504379906,-3.28355142682418));
#25779=CARTESIAN_POINT('Ctrl Pts',(-43.7117878594451,2.11226815661032,-3.58204221900527));
#25780=CARTESIAN_POINT('Ctrl Pts',(-43.724947801425,1.15867261640002,-3.9918383467642));
#25781=CARTESIAN_POINT('Ctrl Pts',(-43.7311919121336,0.655195493564536,
-4.10463443942983));
#25782=CARTESIAN_POINT('Ctrl Pts',(-43.7368750008672,0.143960423897816,
-4.12248716145376));
#25783=CARTESIAN_POINT('',(-43.8559375004336,0.143960423897816,-4.12248716145376));
#25784=CARTESIAN_POINT('Origin',(-43.975,0.,0.));
#25785=CARTESIAN_POINT('Ctrl Pts',(-43.6591154631359,-5.88152861126802E-14,
-4.12499999999999));
#25786=CARTESIAN_POINT('Ctrl Pts',(-43.6589893495955,0.0111341806831491,
-4.12499999999999));
#25787=CARTESIAN_POINT('Ctrl Pts',(-43.6588634832089,0.0222705103512012,
-4.12495492002788));
#25788=CARTESIAN_POINT('Ctrl Pts',(-43.6528491033062,0.555558413132617,
-4.12063563480334));
#25789=CARTESIAN_POINT('Ctrl Pts',(-43.6466866748295,1.07219509882857,-4.01729972547807));
#25790=CARTESIAN_POINT('Ctrl Pts',(-43.6332360135605,2.05777766494,-3.61592783690613));
#25791=CARTESIAN_POINT('Ctrl Pts',(-43.6262179313814,2.51456795578323,-3.31456360783142));
#25792=CARTESIAN_POINT('Ctrl Pts',(-43.6126724826772,3.2842264042745,-2.5536973745261));
#25793=CARTESIAN_POINT('Ctrl Pts',(-43.6066817918365,3.59009962015523,-2.10206847694175));
#25794=CARTESIAN_POINT('Ctrl Pts',(-43.5942516665281,4.00554134652347,-1.118007782556));
#25795=CARTESIAN_POINT('Ctrl Pts',(-43.5876182065664,4.11560219486197,-0.596752694620666));
#25796=CARTESIAN_POINT('Ctrl Pts',(-43.5738241914443,4.13359553106555,0.479812571999722));
#25797=CARTESIAN_POINT('Ctrl Pts',(-43.5667907652833,4.03316101536502,1.02491447200937));
#25798=CARTESIAN_POINT('Ctrl Pts',(-43.5538235392921,3.63344749912529,2.02240331718184));
#25799=CARTESIAN_POINT('Ctrl Pts',(-43.5482445740158,3.34636672711171,2.46857976389889));
#25800=CARTESIAN_POINT('Ctrl Pts',(-43.5353393944105,2.61450760049208,3.23497562268258));
#25801=CARTESIAN_POINT('Ctrl Pts',(-43.5284804597234,2.17426530363052,3.5458826013205));
#25802=CARTESIAN_POINT('Ctrl Pts',(-43.5146565723004,1.18866196397726,3.98760057133189));
#25803=CARTESIAN_POINT('Ctrl Pts',(-43.5078293194862,0.650866351281966,
4.10977587436382));
#25804=CARTESIAN_POINT('Ctrl Pts',(-43.4955762826235,-0.416478607119255,
4.13693051141778));
#25805=CARTESIAN_POINT('Ctrl Pts',(-43.4896521368969,-0.935687040047014,
4.051190919213));
#25806=CARTESIAN_POINT('Ctrl Pts',(-43.4763198279506,-1.93199439036745,
3.68439226432171));
#25807=CARTESIAN_POINT('Ctrl Pts',(-43.4693247754649,-2.39730049356399,
3.40004392262083));
#25808=CARTESIAN_POINT('Ctrl Pts',(-43.4556306941763,-3.19624375915856,
2.66417888234778));
#25809=CARTESIAN_POINT('Ctrl Pts',(-43.4493885733127,-3.52047080129217,
2.21812931962595));
#25810=CARTESIAN_POINT('Ctrl Pts',(-43.4370960977028,-3.96810446840913,
1.24368117175732));
#25811=CARTESIAN_POINT('Ctrl Pts',(-43.4305386941905,-4.09425198481728,
0.727796748705689));
#25812=CARTESIAN_POINT('Ctrl Pts',(-43.416819479703,-4.14684849979684,-0.34414241772645));
#25813=CARTESIAN_POINT('Ctrl Pts',(-43.4097799656186,-4.06473266900419,
-0.890358879991509));
#25814=CARTESIAN_POINT('Ctrl Pts',(-43.3966496446118,-3.69845197366426,
-1.9017366805059));
#25815=CARTESIAN_POINT('Ctrl Pts',(-43.3910360105349,-3.42452061952142,
-2.3596201642345));
#25816=CARTESIAN_POINT('Ctrl Pts',(-43.3782569044449,-2.71636030568324,
-3.14965330502464));
#25817=CARTESIAN_POINT('Ctrl Pts',(-43.3714513328493,-2.28771552358482,
-3.47351143594485));
#25818=CARTESIAN_POINT('Ctrl Pts',(-43.3576250115465,-1.31855718802831,
-3.94656209058349));
#25819=CARTESIAN_POINT('Ctrl Pts',(-43.3507398923813,-0.784984740112883,
-4.08628834955838));
#25820=CARTESIAN_POINT('Ctrl Pts',(-43.3434394408746,-0.159800277789472,
-4.12268075233252));
#25821=CARTESIAN_POINT('Ctrl Pts',(-43.3425200419099,-0.0798625070550304,
-4.12499999999999));
#25822=CARTESIAN_POINT('Ctrl Pts',(-43.3416154631359,-1.12029116405105E-15,
-4.12499999999999));
#25823=CARTESIAN_POINT('Origin',(-44.,0.,0.));
#25824=CARTESIAN_POINT('',(-43.0241154623315,3.55101082989618E-8,-4.12499999999999));
#25825=CARTESIAN_POINT('',(-43.1034904640031,1.43537882654006E-14,-4.12499999999999));
#25826=CARTESIAN_POINT('',(-44.,-5.05166804648282E-16,-4.12499999999999));
#25827=CARTESIAN_POINT('Ctrl Pts',(-43.1034904640031,2.66800470605233E-14,
-4.12499999999999));
#25828=CARTESIAN_POINT('Ctrl Pts',(-43.1052759746021,-0.157637296951777,
-4.12499999999999));
#25829=CARTESIAN_POINT('Ctrl Pts',(-43.1071177918741,-0.315441248402036,
-4.11596406793883));
#25830=CARTESIAN_POINT('Ctrl Pts',(-43.1155801821711,-1.01938953197842,
-4.03477234996318));
#25831=CARTESIAN_POINT('Ctrl Pts',(-43.1226029500698,-1.54803169098638,
-3.86291787270377));
#25832=CARTESIAN_POINT('Ctrl Pts',(-43.1364480328831,-2.48824646386089,
-3.33231706468981));
#25833=CARTESIAN_POINT('Ctrl Pts',(-43.1431392580727,-2.89481536520694,
-2.98592673132087));
#25834=CARTESIAN_POINT('Ctrl Pts',(-43.1556794793951,-3.55911665894801,
-2.15307206131927));
#25835=CARTESIAN_POINT('Ctrl Pts',(-43.1615091733841,-3.80851942528891,
-1.67278633352888));
#25836=CARTESIAN_POINT('Ctrl Pts',(-43.1749294953952,-4.11166775494155,
-0.63658374513006));
#25837=CARTESIAN_POINT('Ctrl Pts',(-43.181960207216,-4.15968428344299,-0.0898630879483996));
#25838=CARTESIAN_POINT('Ctrl Pts',(-43.1955032704882,-4.04319752992879,
0.970567332147449));
#25839=CARTESIAN_POINT('Ctrl Pts',(-43.2019012030249,-3.88760292525187,
1.47511599045853));
#25840=CARTESIAN_POINT('Ctrl Pts',(-43.2137810015111,-3.38549162281178,
2.4191248825152));
#25841=CARTESIAN_POINT('Ctrl Pts',(-43.2204822457843,-3.03593416215933,
2.84548968059295));
#25842=CARTESIAN_POINT('Ctrl Pts',(-43.2342625605633,-2.19802302773201,
3.53167830687168));
#25843=CARTESIAN_POINT('Ctrl Pts',(-43.2412020406226,-1.72003210358548,
3.78755181652603));
#25844=CARTESIAN_POINT('Ctrl Pts',(-43.2543303665285,-0.706898517967219,
4.09741633258318));
#25845=CARTESIAN_POINT('Ctrl Pts',(-43.2599952700414,-0.182841721369498,
4.15392485974037));
#25846=CARTESIAN_POINT('Ctrl Pts',(-43.27258568614,0.882197411269908,4.06641392686791));
#25847=CARTESIAN_POINT('Ctrl Pts',(-43.2795082293,1.41232328103033,3.9139915817091));
#25848=CARTESIAN_POINT('Ctrl Pts',(-43.293326935015,2.36887210151711,3.41849039809921));
#25849=CARTESIAN_POINT('Ctrl Pts',(-43.3000894237945,2.78883430396983,3.08545633642643));
#25850=CARTESIAN_POINT('Ctrl Pts',(-43.3127744739824,3.47957156632881,2.27827258369358));
#25851=CARTESIAN_POINT('Ctrl Pts',(-43.3184504853474,3.74379956401648,1.81160442420162));
#25852=CARTESIAN_POINT('Ctrl Pts',(-43.3316979749886,4.08519911444116,0.790218569659973));
#25853=CARTESIAN_POINT('Ctrl Pts',(-43.3387371374263,4.1537902969791,0.243557244814858));
#25854=CARTESIAN_POINT('Ctrl Pts',(-43.352392196471,4.07577218433711,-0.824265521417086));
#25855=CARTESIAN_POINT('Ctrl Pts',(-43.3588893768645,3.93786891142691,-1.33586304490966));
#25856=CARTESIAN_POINT('Ctrl Pts',(-43.3710773892195,3.46630909135439,-2.30299855020026));
#25857=CARTESIAN_POINT('Ctrl Pts',(-43.3775451400705,3.12810928621691,-2.74482226760805));
#25858=CARTESIAN_POINT('Ctrl Pts',(-43.3913460634929,2.30735339026894,-3.46149660931171));
#25859=CARTESIAN_POINT('Ctrl Pts',(-43.398318482974,1.83605538028894,-3.73292651099064));
#25860=CARTESIAN_POINT('Ctrl Pts',(-43.4106822940254,0.898449640878296,
-4.05119835744849));
#25861=CARTESIAN_POINT('Ctrl Pts',(-43.4158878772981,0.450491851513638,
-4.12499999999999));
#25862=CARTESIAN_POINT('Ctrl Pts',(-43.4209904640031,2.15305958091061E-15,
-4.12499999999999));
#25863=CARTESIAN_POINT('Ctrl Pts',(-43.3416154631359,-1.12029116405105E-15,
-4.12499999999999));
#25864=CARTESIAN_POINT('Ctrl Pts',(-43.3366238909621,0.440690716415442,
-4.12499999999999));
#25865=CARTESIAN_POINT('Ctrl Pts',(-43.3315395690574,0.879083534272734,
-4.05437460853012));
#25866=CARTESIAN_POINT('Ctrl Pts',(-43.3193225167226,1.8093221609183,-3.74590157636243));
#25867=CARTESIAN_POINT('Ctrl Pts',(-43.312357155907,2.28221507838271,-3.47806241162083));
#25868=CARTESIAN_POINT('Ctrl Pts',(-43.2986058700743,3.10428455213175,-2.77079207616584));
#25869=CARTESIAN_POINT('Ctrl Pts',(-43.2921143504653,3.44344052223974,-2.33593029491167));
#25870=CARTESIAN_POINT('Ctrl Pts',(-43.2800569829449,3.92299988165074,-1.3787057721374));
#25871=CARTESIAN_POINT('Ctrl Pts',(-43.2735890934869,4.06635403816314,-0.869202600509911));
#25872=CARTESIAN_POINT('Ctrl Pts',(-43.2599665762459,4.1561992094172,0.196494906175366));
#25873=CARTESIAN_POINT('Ctrl Pts',(-43.2529289889307,4.09391972913349,0.743253780537866));
#25874=CARTESIAN_POINT('Ctrl Pts',(-43.2396277769611,3.76419938548784,1.76923783817601));
#25875=CARTESIAN_POINT('Ctrl Pts',(-43.2339121132508,3.50450765055868,2.24004991540411));
#25876=CARTESIAN_POINT('Ctrl Pts',(-43.2212712597041,2.82188654574836,3.05515937030567));
#25877=CARTESIAN_POINT('Ctrl Pts',(-43.2145299107476,2.40600978151607,3.39236689111578));
#25878=CARTESIAN_POINT('Ctrl Pts',(-43.2006455938717,1.45053478435525,3.90078195707088));
#25879=CARTESIAN_POINT('Ctrl Pts',(-43.1936374133849,0.916266102859524,
4.05963233795626));
#25880=CARTESIAN_POINT('Ctrl Pts',(-43.1809398703271,-0.153985615878453,
4.15512756988326));
#25881=CARTESIAN_POINT('Ctrl Pts',(-43.1752949016246,-0.678687930182376,
4.10221674084147));
#25882=CARTESIAN_POINT('Ctrl Pts',(-43.1621921889391,-1.69380827193884,
3.79929948284872));
#25883=CARTESIAN_POINT('Ctrl Pts',(-43.1552609706994,-2.17323075061218,
3.54693227843849));
#25884=CARTESIAN_POINT('Ctrl Pts',(-43.1414729074834,-3.01571167852317,
2.8669170315091));
#25885=CARTESIAN_POINT('Ctrl Pts',(-43.1347555624722,-3.36829176801628,
2.44302098258961));
#25886=CARTESIAN_POINT('Ctrl Pts',(-43.1228311727003,-3.87691226534231,
1.5028694643996));
#25887=CARTESIAN_POINT('Ctrl Pts',(-43.1164997074165,-4.03602609781071,
0.99979001300251));
#25888=CARTESIAN_POINT('Ctrl Pts',(-43.1029809855698,-4.16018275602907,
-0.0590096082767586));
#25889=CARTESIAN_POINT('Ctrl Pts',(-43.0959531158827,-4.11628346110768,
-0.605652355224156));
#25890=CARTESIAN_POINT('Ctrl Pts',(-43.0824990114904,-3.82085591578393,
-1.64475959424927));
#25891=CARTESIAN_POINT('Ctrl Pts',(-43.0766301501403,-3.57443671439989,
-2.12780920288455));
#25892=CARTESIAN_POINT('Ctrl Pts',(-43.0641191842593,-2.91542104739757,
-2.96574701170689));
#25893=CARTESIAN_POINT('Ctrl Pts',(-43.0574430227019,-2.51155811526016,
-3.31472531301843));
#25894=CARTESIAN_POINT('Ctrl Pts',(-43.0436107066202,-1.57581142100035,
-3.85160952045626));
#25895=CARTESIAN_POINT('Ctrl Pts',(-43.0365845808552,-1.04883828179103,
-4.02716051968696));
#25896=CARTESIAN_POINT('Ctrl Pts',(-43.0279803506855,-0.335775072933513,
-4.11476116179616));
#25897=CARTESIAN_POINT('Ctrl Pts',(-43.0260161096807,-0.167802299982725,
-4.12500000144471));
#25898=CARTESIAN_POINT('Ctrl Pts',(-43.0241154627337,3.55147232455888E-8,
-4.12499999999999));
#25899=CARTESIAN_POINT('Origin',(-44.,0.,0.));
#25900=CARTESIAN_POINT('',(-42.7066154631359,-2.40364051253538E-15,-4.12499999999999));
#25901=CARTESIAN_POINT('',(-42.7859904640031,-1.53620248780821E-14,-4.12499999999999));
#25902=CARTESIAN_POINT('',(-44.,-5.05166804648282E-16,-4.12499999999999));
#25903=CARTESIAN_POINT('Ctrl Pts',(-42.7859904640031,-3.47638584585752E-14,
-4.12499999999999));
#25904=CARTESIAN_POINT('Ctrl Pts',(-42.7888245165898,-0.250209878029857,
-4.12499999999999));
#25905=CARTESIAN_POINT('Ctrl Pts',(-42.7917962670083,-0.500472261515978,
-4.10223490248918));
#25906=CARTESIAN_POINT('Ctrl Pts',(-42.8015560655256,-1.28523165018734,
-3.95760041622189));
#25907=CARTESIAN_POINT('Ctrl Pts',(-42.8085958753329,-1.79778204456973,
-3.75265203123737));
#25908=CARTESIAN_POINT('Ctrl Pts',(-42.8222999930062,-2.69584454212555,
-3.16618068502911));
#25909=CARTESIAN_POINT('Ctrl Pts',(-42.8288428847336,-3.07719487032833,
-2.79699093818034));
#25910=CARTESIAN_POINT('Ctrl Pts',(-42.8411098637959,-3.69279084440484,
-1.9179050173747));
#25911=CARTESIAN_POINT('Ctrl Pts',(-42.8474043707732,-3.9143712156974,-1.41165644113701));
#25912=CARTESIAN_POINT('Ctrl Pts',(-42.8611250097368,-4.14545751488401,
-0.349512587343389));
#25913=CARTESIAN_POINT('Ctrl Pts',(-42.8681149403688,-4.15557646971381,
0.195350538477975));
#25914=CARTESIAN_POINT('Ctrl Pts',(-42.881425017066,-3.96860979414112,1.24006915556839));
#25915=CARTESIAN_POINT('Ctrl Pts',(-42.8873118844221,-3.78019612553688,
1.73139937857128));
#25916=CARTESIAN_POINT('Ctrl Pts',(-42.8996027432266,-3.21734484665115,
2.63867222791108));
#25917=CARTESIAN_POINT('Ctrl Pts',(-42.9064416027748,-2.84011387612309,
3.04099378338463));
#25918=CARTESIAN_POINT('Ctrl Pts',(-42.9202671056224,-1.96109074647784,
3.66803676823795));
#25919=CARTESIAN_POINT('Ctrl Pts',(-42.9271163877112,-1.47064201769888,
3.89070522371206));
#25920=CARTESIAN_POINT('Ctrl Pts',(-42.9399978038948,-0.439333279023981,
4.1351622341229));
#25921=CARTESIAN_POINT('Ctrl Pts',(-42.9455788864246,0.0912667879587264,
4.15743317289483));
#25922=CARTESIAN_POINT('Ctrl Pts',(-42.9585773827393,1.15412200234955,3.99805577246191));
#25923=CARTESIAN_POINT('Ctrl Pts',(-42.9656125412644,1.6748987435772,3.80935121142002));
#25924=CARTESIAN_POINT('Ctrl Pts',(-42.9793934583387,2.59426481170688,3.250194003948));
#25925=CARTESIAN_POINT('Ctrl Pts',(-42.9860130016714,2.98827660915105,2.89208950765888));
#25926=CARTESIAN_POINT('Ctrl Pts',(-42.9984173813874,3.62818198206529,2.03590841524423));
#25927=CARTESIAN_POINT('Ctrl Pts',(-43.0044509665188,3.86374723920393,1.54275460734297));
#25928=CARTESIAN_POINT('Ctrl Pts',(-43.0180248816437,4.13105728843214,0.493320214040006));
#25929=CARTESIAN_POINT('Ctrl Pts',(-43.0250392589146,4.16007352615153,-0.0527898485888066));
#25930=CARTESIAN_POINT('Ctrl Pts',(-43.0384680104133,4.00822866347273,-1.10553865169403));
#25931=CARTESIAN_POINT('Ctrl Pts',(-43.0445811221813,3.83631078108773,-1.60337691310156));
#25932=CARTESIAN_POINT('Ctrl Pts',(-43.056666822505,3.30398722598507,-2.52932488849252));
#25933=CARTESIAN_POINT('Ctrl Pts',(-43.0634400914866,2.94051137861696,-2.94401066815298));
#25934=CARTESIAN_POINT('Ctrl Pts',(-43.0772505199682,2.08171497497243,-3.6012056953707));
#25935=CARTESIAN_POINT('Ctrl Pts',(-43.0841488103069,1.59727264490132,-3.84069566259819));
#25936=CARTESIAN_POINT('Ctrl Pts',(-43.0952134104074,0.727707799486982,
-4.07673776869245));
#25937=CARTESIAN_POINT('Ctrl Pts',(-43.0993641378131,0.364300781693087,
-4.12499999999999));
#25938=CARTESIAN_POINT('Ctrl Pts',(-43.1034904640031,2.68869879372251E-14,
-4.12499999999999));
#25939=CARTESIAN_POINT('Ctrl Pts',(-43.0241154627337,3.55147231723032E-8,
-4.12499999999999));
#25940=CARTESIAN_POINT('Ctrl Pts',(-43.0201000493006,0.354508669064718,
-4.1249999969478));
#25941=CARTESIAN_POINT('Ctrl Pts',(-43.0160674581826,0.708253156444587,
-4.07929759244896));
#25942=CARTESIAN_POINT('Ctrl Pts',(-43.005151345896,1.56964374183415,-3.85201695055881));
#25943=CARTESIAN_POINT('Ctrl Pts',(-42.9982631939178,2.05545173993792,-3.61620389309265));
#25944=CARTESIAN_POINT('Ctrl Pts',(-42.9844481153621,2.91877349526748,-2.96556690220725));
#25945=CARTESIAN_POINT('Ctrl Pts',(-42.9776597934361,3.28530187692224,-2.55355186408069));
#25946=CARTESIAN_POINT('Ctrl Pts',(-42.9655287220031,3.82433839284296,-1.63167264176363));
#25947=CARTESIAN_POINT('Ctrl Pts',(-42.9594706776355,3.99988166706038,-1.13528834876725));
#25948=CARTESIAN_POINT('Ctrl Pts',(-42.9460677647307,4.1595007036321,-0.0842834828703053));
#25949=CARTESIAN_POINT('Ctrl Pts',(-42.9390580901803,4.13466688486896,0.461605819570947));
#25950=CARTESIAN_POINT('Ctrl Pts',(-42.9254511705147,3.87532109108673,1.51389269394917));
#25951=CARTESIAN_POINT('Ctrl Pts',(-42.9193648073432,3.64282907543009,2.00991867577158));
#25952=CARTESIAN_POINT('Ctrl Pts',(-42.9069906288836,3.00829785461101,2.87119235244729));
#25953=CARTESIAN_POINT('Ctrl Pts',(-42.9003875970296,2.61707371796781,3.23179805054191));
#25954=CARTESIAN_POINT('Ctrl Pts',(-42.8866225796335,1.70237454360611,3.79709236858559));
#25955=CARTESIAN_POINT('Ctrl Pts',(-42.8795857432846,1.1833843510517,3.9894355309398));
#25956=CARTESIAN_POINT('Ctrl Pts',(-42.8665510177599,0.121543390730149,
4.15673609487457));
#25957=CARTESIAN_POINT('Ctrl Pts',(-42.8609648298656,-0.409834881232685,
4.13826813090633));
#25958=CARTESIAN_POINT('Ctrl Pts',(-42.8481111837364,-1.44306283468347,
3.90096756669595));
#25959=CARTESIAN_POINT('Ctrl Pts',(-42.8412734251041,-1.93473515675691,
3.68195240576325));
#25960=CARTESIAN_POINT('Ctrl Pts',(-42.8274467266498,-2.81799138172734,
3.06150791209393));
#25961=CARTESIAN_POINT('Ctrl Pts',(-42.8205947213512,-3.19813918176695,
2.66192047922009));
#25962=CARTESIAN_POINT('Ctrl Pts',(-42.8082601062542,-3.76756140231514,
1.75872664932032));
#25963=CARTESIAN_POINT('Ctrl Pts',(-42.8024138241952,-3.95953098506463,
1.26876331708425));
#25964=CARTESIAN_POINT('Ctrl Pts',(-42.7891296672012,-4.15398136719704,
0.22580510709411));
#25965=CARTESIAN_POINT('Ctrl Pts',(-42.7821460098025,-4.14788774154854,
-0.318709272419962));
#25966=CARTESIAN_POINT('Ctrl Pts',(-42.7683949303322,-3.92460064974471,
-1.38349984832726));
#25967=CARTESIAN_POINT('Ctrl Pts',(-42.7620374185745,-3.70603558555749,
-1.89257731912303));
#25968=CARTESIAN_POINT('Ctrl Pts',(-42.7498000358233,-3.09562961199559,
-2.77650993271348));
#25969=CARTESIAN_POINT('Ctrl Pts',(-42.7432741437303,-2.71699806369652,
-3.14799028012294));
#25970=CARTESIAN_POINT('Ctrl Pts',(-42.7295880116923,-1.823544844846,-3.74014401885518));
#25971=CARTESIAN_POINT('Ctrl Pts',(-42.7225481710413,-1.31279735592544,
-3.94848829724771));
#25972=CARTESIAN_POINT('Ctrl Pts',(-42.7126518238129,-0.519869054439207,
-4.10043233476657));
#25973=CARTESIAN_POINT('Ctrl Pts',(-42.7095595751266,-0.259926687862678,
-4.12499999999999));
#25974=CARTESIAN_POINT('Ctrl Pts',(-42.7066154631359,-2.77555756156289E-16,
-4.12499999999999));
#25975=CARTESIAN_POINT('Origin',(-44.,0.,0.));
#25976=CARTESIAN_POINT('',(-42.3891154631359,-2.19547369541817E-15,-4.12499999999999));
#25977=CARTESIAN_POINT('',(-42.4684904640031,1.15782307038377E-14,-4.12499999999999));
#25978=CARTESIAN_POINT('',(-44.,-5.05166804648282E-16,-4.12499999999999));
#25979=CARTESIAN_POINT('Ctrl Pts',(-42.4684904640031,2.16493489801906E-14,
-4.12499999999999));
#25980=CARTESIAN_POINT('Ctrl Pts',(-42.4724362677784,-0.348363007083697,
-4.12499999999999));
#25981=CARTESIAN_POINT('Ctrl Pts',(-42.4766406552945,-0.696090583128804,
-4.08086874866564));
#25982=CARTESIAN_POINT('Ctrl Pts',(-42.4877762594709,-1.56016154950479,
-3.85695389900486));
#25983=CARTESIAN_POINT('Ctrl Pts',(-42.4948011956894,-2.05355245920538,
-3.61844142857051));
#25984=CARTESIAN_POINT('Ctrl Pts',(-42.5082974697846,-2.90361541835705,
-2.97620717943818));
#25985=CARTESIAN_POINT('Ctrl Pts',(-42.5145704841859,-3.25697037235858,
-2.58474681575524));
#25986=CARTESIAN_POINT('Ctrl Pts',(-42.5265356262334,-3.81079775100409,
-1.67080256498323));
#25987=CARTESIAN_POINT('Ctrl Pts',(-42.5332674465324,-3.99825409380244,
-1.15226487328355));
#25988=CARTESIAN_POINT('Ctrl Pts',(-42.5470620051222,-4.15891699238856,
-0.0818960292318208));
#25989=CARTESIAN_POINT('Ctrl Pts',(-42.5539853576718,-4.13432363969937,
0.458986168573618));
#25990=CARTESIAN_POINT('Ctrl Pts',(-42.5670644201357,-3.8826671044889,1.48794463240853));
#25991=CARTESIAN_POINT('Ctrl Pts',(-42.5726933681788,-3.66296944596519,
1.9676726110332));
#25992=CARTESIAN_POINT('Ctrl Pts',(-42.5854241355369,-3.03953589276337,
2.84270545807145));
#25993=CARTESIAN_POINT('Ctrl Pts',(-42.5924363794386,-2.63269427749126,
3.22314544875958));
#25994=CARTESIAN_POINT('Ctrl Pts',(-42.6063116669039,-1.71170506016576,
3.79035212504384));
#25995=CARTESIAN_POINT('Ctrl Pts',(-42.6130408464765,-1.21088314117952,
3.97875255600666));
#25996=CARTESIAN_POINT('Ctrl Pts',(-42.6256567611582,-0.162105593265999,
4.15619753914953));
#25997=CARTESIAN_POINT('Ctrl Pts',(-42.6313976429439,0.376227252487634,
4.1423075269595));
#25998=CARTESIAN_POINT('Ctrl Pts',(-42.6447287902611,1.42854328412835,3.90787423126925));
#25999=CARTESIAN_POINT('Ctrl Pts',(-42.6517650968985,1.93143647261353,3.68534496256726));
#26000=CARTESIAN_POINT('Ctrl Pts',(-42.6653685882037,2.80503073811873,3.06956393080499));
#26001=CARTESIAN_POINT('Ctrl Pts',(-42.671819676093,3.17202630260548,2.68862024117154));
#26002=CARTESIAN_POINT('Ctrl Pts',(-42.683833022173,3.75560589010962,1.79143439236175));
#26003=CARTESIAN_POINT('Ctrl Pts',(-42.6903743154332,3.95951954397787,1.27907690494286));
#26004=CARTESIAN_POINT('Ctrl Pts',(-42.7041335991802,4.15449872894309,0.212657859332945));
#26005=CARTESIAN_POINT('Ctrl Pts',(-42.7110928844457,4.14679344901288,-0.330437355567603));
#26006=CARTESIAN_POINT('Ctrl Pts',(-42.7242864692273,3.92666265703818,-1.36722768807397));
#26007=CARTESIAN_POINT('Ctrl Pts',(-42.730014556812,3.72237025880694,-1.85255123012292));
#26008=CARTESIAN_POINT('Ctrl Pts',(-42.7424993207356,3.13022561702276,-2.7414689395802));
#26009=CARTESIAN_POINT('Ctrl Pts',(-42.7493940681355,2.7401188756063,-3.13140622944548));
#26010=CARTESIAN_POINT('Ctrl Pts',(-42.7632192418648,1.84256598940375,-3.7287469907487));
#26011=CARTESIAN_POINT('Ctrl Pts',(-42.7700144866968,1.34685573561633,-3.93504619916284));
#26012=CARTESIAN_POINT('Ctrl Pts',(-42.7797493595055,0.553324077123309,
-4.09715985949721));
#26013=CARTESIAN_POINT('Ctrl Pts',(-42.7828564229322,0.276694948344091,
-4.12499999999999));
#26014=CARTESIAN_POINT('Ctrl Pts',(-42.7859904640031,-3.44139441956932E-14,
-4.12499999999999));
#26015=CARTESIAN_POINT('Ctrl Pts',(-42.7066154631359,-1.12029116405105E-15,
-4.12499999999999));
#26016=CARTESIAN_POINT('Ctrl Pts',(-42.7035833111296,0.267699472910892,
-4.12499999999999));
#26017=CARTESIAN_POINT('Ctrl Pts',(-42.7005816690409,0.535380873838965,
-4.09894073043939));
#26018=CARTESIAN_POINT('Ctrl Pts',(-42.6909831651212,1.32075710604345,-3.94383594341831));
#26019=CARTESIAN_POINT('Ctrl Pts',(-42.6842000643013,1.81750192394942,-3.74097880526701));
#26020=CARTESIAN_POINT('Ctrl Pts',(-42.670376808526,2.71880892727669,-3.14992802416122));
#26021=CARTESIAN_POINT('Ctrl Pts',(-42.6634712901854,3.11156008564056,-2.76263824749651));
#26022=CARTESIAN_POINT('Ctrl Pts',(-42.6509464481592,3.70981792363214,-1.87760808468546));
#26023=CARTESIAN_POINT('Ctrl Pts',(-42.6452442989327,3.91743447999407,-1.39351081816239));
#26024=CARTESIAN_POINT('Ctrl Pts',(-42.6320753195121,4.14442330981951,-0.358400222540147));
#26025=CARTESIAN_POINT('Ctrl Pts',(-42.6251232878707,4.15580827963938,0.184257705315122));
#26026=CARTESIAN_POINT('Ctrl Pts',(-42.6113554379963,3.96828355277432,1.25160522660637));
#26027=CARTESIAN_POINT('Ctrl Pts',(-42.604754990877,3.76794253452459,1.76532634455065));
#26028=CARTESIAN_POINT('Ctrl Pts',(-42.5927925942258,3.1908272637106,2.66620997745897));
#26029=CARTESIAN_POINT('Ctrl Pts',(-42.5863610425975,2.82679081582617,3.04947508457934));
#26030=CARTESIAN_POINT('Ctrl Pts',(-42.5727799861511,1.95827987055198,3.67109128614302));
#26031=CARTESIAN_POINT('Ctrl Pts',(-42.565745495969,1.45741866387244,3.89714054600239));
#26032=CARTESIAN_POINT('Ctrl Pts',(-42.5523803067902,0.406356146781749,
4.13958379346201));
#26033=CARTESIAN_POINT('Ctrl Pts',(-42.5466079711067,-0.132845589110581,
4.15735835990101));
#26034=CARTESIAN_POINT('Ctrl Pts',(-42.5340206983149,-1.18339757627937,
3.98696638339271));
#26035=CARTESIAN_POINT('Ctrl Pts',(-42.5273057032173,-1.68517010770252,
3.80217383029169));
#26036=CARTESIAN_POINT('Ctrl Pts',(-42.5134413562945,-2.60948276667548,
3.2418951599226));
#26037=CARTESIAN_POINT('Ctrl Pts',(-42.5064248136894,-3.01874389665988,
2.86469484965848));
#26038=CARTESIAN_POINT('Ctrl Pts',(-42.4936563305807,-3.64856784200123,
1.99434066474303));
#26039=CARTESIAN_POINT('Ctrl Pts',(-42.4880429459267,-3.87188615970388,
1.51589628663844));
#26040=CARTESIAN_POINT('Ctrl Pts',(-42.4749909574358,-4.13085568628257,
0.488794224764731));
#26041=CARTESIAN_POINT('Ctrl Pts',(-42.4680768830096,-4.15935489999998,
-0.0515006725587147));
#26042=CARTESIAN_POINT('Ctrl Pts',(-42.4542756513481,-4.00666787072579,
-1.12266854151268));
#26043=CARTESIAN_POINT('Ctrl Pts',(-42.4475277137696,-3.82304289047505,
-1.64259717952674));
#26044=CARTESIAN_POINT('Ctrl Pts',(-42.4355164062618,-3.27611316122999,
-2.56038321995924));
#26045=CARTESIAN_POINT('Ctrl Pts',(-42.4293069356349,-2.9258902950147,-2.95426188547286));
#26046=CARTESIAN_POINT('Ctrl Pts',(-42.4158363220833,-2.08128414995036,
-3.60249813982044));
#26047=CARTESIAN_POINT('Ctrl Pts',(-42.408815096909,-1.59014509167932,-3.84462953161962));
#26048=CARTESIAN_POINT('Ctrl Pts',(-42.3975278013324,-0.717744544535816,
-4.07806610689559));
#26049=CARTESIAN_POINT('Ctrl Pts',(-42.3931846180739,-0.359253305846238,
-4.12499999999999));
#26050=CARTESIAN_POINT('Ctrl Pts',(-42.3891154631359,-1.2490009027033E-14,
-4.12499999999999));
#26051=CARTESIAN_POINT('Origin',(-44.,0.,0.));
#26052=CARTESIAN_POINT('',(-42.0716154631359,2.62705756779736E-15,-4.12499999999999));
#26053=CARTESIAN_POINT('',(-42.1509904640031,1.22027311551893E-14,-4.12499999999999));
#26054=CARTESIAN_POINT('',(-44.,-5.05166804648282E-16,-4.12499999999999));
#26055=CARTESIAN_POINT('Ctrl Pts',(-42.1509904640031,3.17801340798951E-14,
-4.12499999999999));
#26056=CARTESIAN_POINT('Ctrl Pts',(-42.1560338924339,-0.445268947525859,
-4.12499999999999));
#26057=CARTESIAN_POINT('Ctrl Pts',(-42.1614864674767,-0.888322840384305,
-4.05289790512554));
#26058=CARTESIAN_POINT('Ctrl Pts',(-42.1739587071193,-1.82280109361283,
-3.73946011707928));
#26059=CARTESIAN_POINT('Ctrl Pts',(-42.1809364412098,-2.29532167022266,
-3.46953387089725));
#26060=CARTESIAN_POINT('Ctrl Pts',(-42.1941972499297,-3.09660567355616,
-2.77465727096019));
#26061=CARTESIAN_POINT('Ctrl Pts',(-42.2000095838757,-3.42229302213132,
-2.36126943593959));
#26062=CARTESIAN_POINT('Ctrl Pts',(-42.2123833088279,-3.91364098116501,
-1.41327377823633));
#26063=CARTESIAN_POINT('Ctrl Pts',(-42.2192468040062,-4.06617713874996,
-0.883245970453483));
#26064=CARTESIAN_POINT('Ctrl Pts',(-42.2330739520629,-4.15483875880001,
0.192179200922925));
#26065=CARTESIAN_POINT('Ctrl Pts',(-42.2399010836908,-4.09529222310576,
0.726776732738759));
#26066=CARTESIAN_POINT('Ctrl Pts',(-42.2527296541061,-3.77776018814276,
1.73849717190354));
#26067=CARTESIAN_POINT('Ctrl Pts',(-42.2583228562987,-3.52474092831486,
2.2068180825215));
#26068=CARTESIAN_POINT('Ctrl Pts',(-42.2713900111586,-2.84321758139603,
3.03837146446667));
#26069=CARTESIAN_POINT('Ctrl Pts',(-42.2784280439159,-2.41513573679348,
3.38861360283517));
#26070=CARTESIAN_POINT('Ctrl Pts',(-42.2921781579391,-1.46558462246781,
3.89169829027523));
#26071=CARTESIAN_POINT('Ctrl Pts',(-42.298766051037,-0.957005192665014,
4.04690043324374));
#26072=CARTESIAN_POINT('Ctrl Pts',(-42.3111128479386,0.10769051217861,4.15928298587356));
#26073=CARTESIAN_POINT('Ctrl Pts',(-42.3172493225262,0.654372363406386,
4.10889740066407));
#26074=CARTESIAN_POINT('Ctrl Pts',(-42.3308858004633,1.69395759783205,3.79982275752029));
#26075=CARTESIAN_POINT('Ctrl Pts',(-42.3378908816764,2.17704339310721,3.5452259825536));
#26076=CARTESIAN_POINT('Ctrl Pts',(-42.3512702445266,3.00254148378252,2.87620430103972));
#26077=CARTESIAN_POINT('Ctrl Pts',(-42.3572809620275,3.34187630402635,2.47379412796274));
#26078=CARTESIAN_POINT('Ctrl Pts',(-42.3694530362566,3.86447672600527,1.54261864147942));
#26079=CARTESIAN_POINT('Ctrl Pts',(-42.3762546983053,4.03453426683527,1.01802569478419));
#26080=CARTESIAN_POINT('Ctrl Pts',(-42.3900733439701,4.15913036951586,-0.055481427931184));
#26081=CARTESIAN_POINT('Ctrl Pts',(-42.3969519954047,4.1169424906266,-0.593491341014654));
#26082=CARTESIAN_POINT('Ctrl Pts',(-42.4099073092143,3.83225847614284,-1.61395072119891));
#26083=CARTESIAN_POINT('Ctrl Pts',(-42.4154887279345,3.59605813030624,-2.08791930193469));
#26084=CARTESIAN_POINT('Ctrl Pts',(-42.4283891662422,2.943644797198,-2.94153392581003));
#26085=CARTESIAN_POINT('Ctrl Pts',(-42.4354180316776,2.52599193930369,-3.30711739042688));
#26086=CARTESIAN_POINT('Ctrl Pts',(-42.4492381287215,1.59028508813065,-3.84265224811036));
#26087=CARTESIAN_POINT('Ctrl Pts',(-42.4559002985671,1.08534260792206,-4.01460106544558));
#26088=CARTESIAN_POINT('Ctrl Pts',(-42.4642898645937,0.375169285999567,
-4.1122171789071));
#26089=CARTESIAN_POINT('Ctrl Pts',(-42.4663667894089,0.187492766960302,
-4.12499999999999));
#26090=CARTESIAN_POINT('Ctrl Pts',(-42.4684904640031,2.09704502270805E-14,
-4.12499999999999));
#26091=CARTESIAN_POINT('Ctrl Pts',(-42.3891154631359,-1.1763057222536E-14,
-4.12499999999999));
#26092=CARTESIAN_POINT('Ctrl Pts',(-42.3871013770239,0.177817533376489,
-4.12499999999999));
#26093=CARTESIAN_POINT('Ctrl Pts',(-42.385134084848,0.355821541514001,-4.11350241751702));
#26094=CARTESIAN_POINT('Ctrl Pts',(-42.3768891234525,1.05664824774418,-4.02220037883837));
#26095=CARTESIAN_POINT('Ctrl Pts',(-42.3702430602757,1.56245378510728,-3.85400208227205));
#26096=CARTESIAN_POINT('Ctrl Pts',(-42.3564374347192,2.50136014959374,-3.32571631658645));
#26097=CARTESIAN_POINT('Ctrl Pts',(-42.3494058416175,2.92139877157236,-2.96354962449462));
#26098=CARTESIAN_POINT('Ctrl Pts',(-42.336467544458,3.58036382231714,-2.11485078686789));
#26099=CARTESIAN_POINT('Ctrl Pts',(-42.330888673688,3.8203268224177,-1.6421639770986));
#26100=CARTESIAN_POINT('Ctrl Pts',(-42.3179616762174,4.11243104906792,-0.623654159522199));
#26101=CARTESIAN_POINT('Ctrl Pts',(-42.311094051705,4.15855387560653,-0.086366937965185));
#26102=CARTESIAN_POINT('Ctrl Pts',(-42.2972721364892,4.04207283103092,0.987678594684015));
#26103=CARTESIAN_POINT('Ctrl Pts',(-42.2904558347728,3.87595592604241,1.51355104947175));
#26104=CARTESIAN_POINT('Ctrl Pts',(-42.2782378352712,3.36039808868393,2.44855465216588));
#26105=CARTESIAN_POINT('Ctrl Pts',(-42.2722773522877,3.0241706380018,2.8534361254441));
#26106=CARTESIAN_POINT('Ctrl Pts',(-42.2589245903854,2.2041621677276,3.52836536376145));
#26107=CARTESIAN_POINT('Ctrl Pts',(-42.2519250414944,1.72343714359835,3.78648349673181));
#26108=CARTESIAN_POINT('Ctrl Pts',(-42.2382557634832,0.685447014643934,
4.10400433986152));
#26109=CARTESIAN_POINT('Ctrl Pts',(-42.2320604506867,0.137790688399652,
4.15856861996258));
#26110=CARTESIAN_POINT('Ctrl Pts',(-42.2197444246986,-0.928622284584786,
4.05346076698241));
#26111=CARTESIAN_POINT('Ctrl Pts',(-42.2131737298568,-1.43792916326425,
3.90195270202446));
#26112=CARTESIAN_POINT('Ctrl Pts',(-42.1994409049684,-2.39038155574977,
3.40605431517219));
#26113=CARTESIAN_POINT('Ctrl Pts',(-42.1924018892718,-2.82068666982909,
3.05922555831872));
#26114=CARTESIAN_POINT('Ctrl Pts',(-42.1792987632596,-3.50858330700064,
2.23258010552681));
#26115=CARTESIAN_POINT('Ctrl Pts',(-42.1736950335671,-3.76532151402767,
1.76548129801672));
#26116=CARTESIAN_POINT('Ctrl Pts',(-42.1608945290857,-4.09000552243583,
0.755700256903659));
#26117=CARTESIAN_POINT('Ctrl Pts',(-42.1540795347079,-4.15330895456272,
0.221918240168212));
#26118=CARTESIAN_POINT('Ctrl Pts',(-42.1402525799222,-4.07247098359919,
-0.853765063861801));
#26119=CARTESIAN_POINT('Ctrl Pts',(-42.1333766474844,-3.92377409583911,
-1.38489705152091));
#26120=CARTESIAN_POINT('Ctrl Pts',(-42.120959597757,-3.43925693052631,-2.33651059002945));
#26121=CARTESIAN_POINT('Ctrl Pts',(-42.1151822829565,-3.11650566204604,
-2.75230237631966));
#26122=CARTESIAN_POINT('Ctrl Pts',(-42.1019475386014,-2.32046290297941,
-3.45270850167069));
#26123=CARTESIAN_POINT('Ctrl Pts',(-42.0949767153039,-1.85027981688563,
-3.72588343508057));
#26124=CARTESIAN_POINT('Ctrl Pts',(-42.0823642419539,-0.908829747591119,
-4.04949405600422));
#26125=CARTESIAN_POINT('Ctrl Pts',(-42.0767765678079,-0.455658224733047,
-4.12499999999999));
#26126=CARTESIAN_POINT('Ctrl Pts',(-42.0716154631359,1.06858966120171E-14,
-4.12499999999999));
#26127=CARTESIAN_POINT('Origin',(-44.,0.,0.));
#26128=CARTESIAN_POINT('',(-41.7541154631073,1.26320085361692E-9,-4.12499999999999));
#26129=CARTESIAN_POINT('',(-41.8334904640031,-3.97348897155563E-14,-4.12499999999999));
#26130=CARTESIAN_POINT('',(-44.,-5.05166804648282E-16,-4.12499999999999));
#26131=CARTESIAN_POINT('Ctrl Pts',(-41.8334904640031,-7.8687056870308E-14,
-4.12499999999999));
#26132=CARTESIAN_POINT('Ctrl Pts',(-41.8395591778476,-0.535788276456958,
-4.12499999999998));
#26133=CARTESIAN_POINT('Ctrl Pts',(-41.8461999805038,-1.06657900485524,
-4.02060928412677));
#26134=CARTESIAN_POINT('Ctrl Pts',(-41.859877854739,-2.0583164902902,-3.61467252212009));
#26135=CARTESIAN_POINT('Ctrl Pts',(-41.866783485758,-2.50979563480639,-3.31714535243961));
#26136=CARTESIAN_POINT('Ctrl Pts',(-41.8798115324135,-3.26517178664293,
-2.57457729607812));
#26137=CARTESIAN_POINT('Ctrl Pts',(-41.8854135929961,-3.56528624481668,
-2.13974936930175));
#26138=CARTESIAN_POINT('Ctrl Pts',(-41.8982151485474,-3.9977239376065,-1.15632561685152));
#26139=CARTESIAN_POINT('Ctrl Pts',(-41.9052351811761,-4.11621596943027,
-0.612898998358878));
#26140=CARTESIAN_POINT('Ctrl Pts',(-41.9190893201413,-4.13252385019637,
0.467158119454977));
#26141=CARTESIAN_POINT('Ctrl Pts',(-41.9257915479999,-4.03850430093581,
0.993216947518014));
#26142=CARTESIAN_POINT('Ctrl Pts',(-41.9383534078591,-3.65461681773415,
1.98645107418684));
#26143=CARTESIAN_POINT('Ctrl Pts',(-41.9441558529599,-3.36625086906328,
2.44347504257847));
#26144=CARTESIAN_POINT('Ctrl Pts',(-41.9575509421477,-2.62518032277939,
3.22797313494093));
#26145=CARTESIAN_POINT('Ctrl Pts',(-41.964583513613,-2.17720829183821,3.54558094845617));
#26146=CARTESIAN_POINT('Ctrl Pts',(-41.978144146734,-1.2024384117774,3.9804339500067));
#26147=CARTESIAN_POINT('Ctrl Pts',(-41.9845581524079,-0.688055081347689,
4.10076853475202));
#26148=CARTESIAN_POINT('Ctrl Pts',(-41.9964750015311,0.380622650465051,
4.14353186971007));
#26149=CARTESIAN_POINT('Ctrl Pts',(-42.0031297052446,0.925132281569847,
4.05683177438524));
#26150=CARTESIAN_POINT('Ctrl Pts',(-42.0169046083988,1.94061878465416,3.67944938583939));
#26151=CARTESIAN_POINT('Ctrl Pts',(-42.0238499588673,2.40290186475778,3.3956463027297));
#26152=CARTESIAN_POINT('Ctrl Pts',(-42.0369970178963,3.18150757612987,2.67700544892334));
#26153=CARTESIAN_POINT('Ctrl Pts',(-42.0426782231437,3.49452654137339,2.25313763786531));
#26154=CARTESIAN_POINT('Ctrl Pts',(-42.0552385214842,3.95614015023096,1.28955085881659));
#26155=CARTESIAN_POINT('Ctrl Pts',(-42.0621533383092,4.09194949567983,0.754935835501052));
#26156=CARTESIAN_POINT('Ctrl Pts',(-42.0759743533171,4.14665431899328,-0.321196753876167));
#26157=CARTESIAN_POINT('Ctrl Pts',(-42.0827464244384,4.07085950337766,-0.852066953666844));
#26158=CARTESIAN_POINT('Ctrl Pts',(-42.0954519040899,3.72226707730659,-1.85527093258268));
#26159=CARTESIAN_POINT('Ctrl Pts',(-42.1011117951717,3.45294113962082,-2.31829704960152));
#26160=CARTESIAN_POINT('Ctrl Pts',(-42.1143341632307,2.74365561441163,-3.12825399866998));
#26161=CARTESIAN_POINT('Ctrl Pts',(-42.1213737511663,2.30605190529893,-3.46348674000982));
#26162=CARTESIAN_POINT('Ctrl Pts',(-42.135043338992,1.34421224947164,-3.93505999849845));
#26163=CARTESIAN_POINT('Ctrl Pts',(-42.1415538466163,0.832648315696499,
-4.07410229519049));
#26164=CARTESIAN_POINT('Ctrl Pts',(-42.1486923346059,0.205876506656136,
-4.12115129696902));
#26165=CARTESIAN_POINT('Ctrl Pts',(-42.1498251835423,0.102879065588091,
-4.12499999999999));
#26166=CARTESIAN_POINT('Ctrl Pts',(-42.1509904640031,3.22433800653442E-14,
-4.12499999999999));
#26167=CARTESIAN_POINT('Ctrl Pts',(-42.0716154631359,1.00826204764594E-14,
-4.12499999999999));
#26168=CARTESIAN_POINT('Ctrl Pts',(-42.0706071354656,0.0890221813736162,
-4.12499999999999));
#26169=CARTESIAN_POINT('Ctrl Pts',(-42.0696256589146,0.17813940412384,-4.12211823705744));
#26170=CARTESIAN_POINT('Ctrl Pts',(-42.0626886542998,0.7909332714484,-4.08233867750673));
#26171=CARTESIAN_POINT('Ctrl Pts',(-42.0562052748367,1.30338169855081,-3.94870250210379));
#26172=CARTESIAN_POINT('Ctrl Pts',(-42.0425654464095,2.26910007257139,-3.48771418943761));
#26173=CARTESIAN_POINT('Ctrl Pts',(-42.0355269191161,2.7097718068153,-3.15754733837929));
#26174=CARTESIAN_POINT('Ctrl Pts',(-42.022253867818,3.42827956248434,-2.35489338257773));
#26175=CARTESIAN_POINT('Ctrl Pts',(-42.0165598775598,3.70308685011076,-1.89361285033071));
#26176=CARTESIAN_POINT('Ctrl Pts',(-42.003895768798,4.06194662621669,-0.89327726827948));
#26177=CARTESIAN_POINT('Ctrl Pts',(-41.9971432275796,4.14307116392663,-0.363744288221829));
#26178=CARTESIAN_POINT('Ctrl Pts',(-41.9833272568024,4.09957329739581,0.712386205342942));
#26179=CARTESIAN_POINT('Ctrl Pts',(-41.9763970206415,3.96932046878808,1.24839797888657));
#26180=CARTESIAN_POINT('Ctrl Pts',(-41.9637759771424,3.51757530187574,2.21706751039052));
#26181=CARTESIAN_POINT('Ctrl Pts',(-41.9581262385893,3.20869952870754,2.64442330263496));
#26182=CARTESIAN_POINT('Ctrl Pts',(-41.9450170702117,2.43754139377463,3.37077950978567));
#26183=CARTESIAN_POINT('Ctrl Pts',(-41.938083744251,1.97868840678086,3.65903706703988));
#26184=CARTESIAN_POINT('Ctrl Pts',(-41.9242975634932,0.967763055249048,
4.04687030811766));
#26185=CARTESIAN_POINT('Ctrl Pts',(-41.9175842347531,0.424208048029082,
4.13929740023204));
#26186=CARTESIAN_POINT('Ctrl Pts',(-41.9056710388727,-0.644320389458257,
4.10779781125427));
#26187=CARTESIAN_POINT('Ctrl Pts',(-41.8993231337814,-1.15943347937385,
3.99310500027776));
#26188=CARTESIAN_POINT('Ctrl Pts',(-41.8857982796435,-2.13785287067713,
3.56935563619536));
#26189=CARTESIAN_POINT('Ctrl Pts',(-41.8787696603756,-2.58881238302563,
3.25711017274507));
#26190=CARTESIAN_POINT('Ctrl Pts',(-41.8653240099461,-3.33939203076905,
2.48039210939859));
#26191=CARTESIAN_POINT('Ctrl Pts',(-41.8594652417615,-3.63353898381416,
2.02516037260728));
#26192=CARTESIAN_POINT('Ctrl Pts',(-41.8469469235392,-4.02793962295403,
1.03495537794674));
#26193=CARTESIAN_POINT('Ctrl Pts',(-41.8402669562126,-4.12733191964218,
0.510445256955648));
#26194=CARTESIAN_POINT('Ctrl Pts',(-41.826431375729,-4.12249034620183,-0.56856470653867));
#26195=CARTESIAN_POINT('Ctrl Pts',(-41.8194060573837,-4.01002352305216,
-1.11261401728585));
#26196=CARTESIAN_POINT('Ctrl Pts',(-41.8065486818142,-3.58848388940988,
-2.10077231492132));
#26197=CARTESIAN_POINT('Ctrl Pts',(-41.8009607349585,-3.29273067922381,
-2.53936740460541));
#26198=CARTESIAN_POINT('Ctrl Pts',(-41.7879735316739,-2.54522144101839,
-3.28994919264909));
#26199=CARTESIAN_POINT('Ctrl Pts',(-41.7810828091145,-2.0974692024319,-3.59201019840101));
#26200=CARTESIAN_POINT('Ctrl Pts',(-41.7672688239022,-1.10147983510762,
-4.01255069242754));
#26201=CARTESIAN_POINT('Ctrl Pts',(-41.7604842356396,-0.561200380517341,
-4.12297039185286));
#26202=CARTESIAN_POINT('Ctrl Pts',(-41.7542297015537,-0.0100808504658389,
-4.12499076228453));
#26203=CARTESIAN_POINT('Ctrl Pts',(-41.7541725520838,-0.00504020946799272,
-4.12500000000308));
#26204=CARTESIAN_POINT('Ctrl Pts',(-41.7541154631073,2.52640221240065E-9,
-4.12499999999999));
#26205=CARTESIAN_POINT('Origin',(-44.,0.,0.));
#26206=CARTESIAN_POINT('',(-41.4366154631359,1.78571668194861E-15,-4.12499999999999));
#26207=CARTESIAN_POINT('',(-41.5159904640031,-7.9070507400718E-15,-4.12499999999999));
#26208=CARTESIAN_POINT('',(-44.,-5.05166804648282E-16,-4.12499999999999));
#26209=CARTESIAN_POINT('Ctrl Pts',(-41.5159904640031,-1.18330754202892E-14,
-4.12499999999999));
#26210=CARTESIAN_POINT('Ctrl Pts',(-41.5169064666755,-0.0808710882830204,
-4.12499999999999));
#26211=CARTESIAN_POINT('Ctrl Pts',(-41.5178376612464,-0.161818913602757,
-4.12262180362065));
#26212=CARTESIAN_POINT('Ctrl Pts',(-41.525152401119,-0.787988831146203,
-4.08571028062563));
#26213=CARTESIAN_POINT('Ctrl Pts',(-41.5320387340023,-1.32145965265631,
-3.94559136003377));
#26214=CARTESIAN_POINT('Ctrl Pts',(-41.5458649386386,-2.29023705263989,
-3.47184364151419));
#26215=CARTESIAN_POINT('Ctrl Pts',(-41.5526692345746,-2.71861702121608,
-3.14769928392844));
#26216=CARTESIAN_POINT('Ctrl Pts',(-41.5654454686437,-3.42624217444751,
-2.35713653314498));
#26217=CARTESIAN_POINT('Ctrl Pts',(-41.5710605547243,-3.69987605959061,
-1.89898547979264));
#26218=CARTESIAN_POINT('Ctrl Pts',(-41.5841945105728,-4.06539635765999,
-0.887297606981464));
#26219=CARTESIAN_POINT('Ctrl Pts',(-41.5912340750953,-4.14709738387759,
-0.341062725244499));
#26220=CARTESIAN_POINT('Ctrl Pts',(-41.6049514347675,-4.0937195899075,0.730759047958374));
#26221=CARTESIAN_POINT('Ctrl Pts',(-41.6115070426618,-3.96720999099781,
1.24651605651722));
#26222=CARTESIAN_POINT('Ctrl Pts',(-41.6237963514478,-3.51884470746436,
2.22074273986629));
#26223=CARTESIAN_POINT('Ctrl Pts',(-41.6300448827958,-3.19419463151977,
2.66666423168129));
#26224=CARTESIAN_POINT('Ctrl Pts',(-41.6437422794425,-2.39458481918784,
3.40195027359171));
#26225=CARTESIAN_POINT('Ctrl Pts',(-41.6507367100721,-1.92909112707186,
3.6859069333138));
#26226=CARTESIAN_POINT('Ctrl Pts',(-41.6640662626243,-0.932543250535931,
4.05191519173872));
#26227=CARTESIAN_POINT('Ctrl Pts',(-41.6699856615776,-0.413272813762911,
4.13725146996676));
#26228=CARTESIAN_POINT('Ctrl Pts',(-41.6822434024603,0.654048294593352,
4.109270905025));
#26229=CARTESIAN_POINT('Ctrl Pts',(-41.6890721110328,1.19175078806432,3.98667875081201));
#26230=CARTESIAN_POINT('Ctrl Pts',(-41.702896228521,2.17697664219642,3.54421263294516));
#26231=CARTESIAN_POINT('Ctrl Pts',(-41.7097539781292,2.61694886463819,3.23299449297784));
#26232=CARTESIAN_POINT('Ctrl Pts',(-41.7226562142323,3.34824990507222,2.46603777649558));
#26233=CARTESIAN_POINT('Ctrl Pts',(-41.7282353282386,3.63502138046449,2.01958879815716));
#26234=CARTESIAN_POINT('Ctrl Pts',(-41.7412064410462,4.03395292401031,1.02176947315805));
#26235=CARTESIAN_POINT('Ctrl Pts',(-41.7482400967005,4.13395732363673,0.47663465262452));
#26236=CARTESIAN_POINT('Ctrl Pts',(-41.7620325149337,4.11514927403033,-0.599834506646873));
#26237=CARTESIAN_POINT('Ctrl Pts',(-41.7686642617806,4.00470855990209,-1.12096923636333));
#26238=CARTESIAN_POINT('Ctrl Pts',(-41.7810912029171,3.58851334733966,-2.10480787679789));
#26239=CARTESIAN_POINT('Ctrl Pts',(-41.7870870932464,3.28221629689906,-2.55630723943552));
#26240=CARTESIAN_POINT('Ctrl Pts',(-41.8006360790771,2.51187359056085,-3.31659875348705));
#26241=CARTESIAN_POINT('Ctrl Pts',(-41.8076537182903,2.05487827683795,-3.61756971572469));
#26242=CARTESIAN_POINT('Ctrl Pts',(-41.8211016757378,1.06904147596912,-4.01813700315628));
#26243=CARTESIAN_POINT('Ctrl Pts',(-41.8272578864661,0.552347994909614,
-4.12106421930381));
#26244=CARTESIAN_POINT('Ctrl Pts',(-41.8332625189997,0.0201441818758197,
-4.12496311665681));
#26245=CARTESIAN_POINT('Ctrl Pts',(-41.8333763904363,0.0100712080537732,
-4.12499999999999));
#26246=CARTESIAN_POINT('Ctrl Pts',(-41.8334904640031,-7.85254087802035E-14,
-4.12499999999999));
#26247=CARTESIAN_POINT('Ctrl Pts',(-41.7541154631073,2.52640221240065E-9,
-4.12499999999999));
#26248=CARTESIAN_POINT('Ctrl Pts',(-41.7482626432124,0.516727659373442,
-4.12499999968352));
#26249=CARTESIAN_POINT('Ctrl Pts',(-41.7422293800106,1.02893702726848,-4.02790594356507));
#26250=CARTESIAN_POINT('Ctrl Pts',(-41.7288835687061,2.01365979063146,-3.64058183567956));
#26251=CARTESIAN_POINT('Ctrl Pts',(-41.7218726813988,2.47352462425983,-3.3451962913757));
#26252=CARTESIAN_POINT('Ctrl Pts',(-41.7082739814623,3.25354692617725,-2.59308227027601));
#26253=CARTESIAN_POINT('Ctrl Pts',(-41.7022010727125,3.56586474073121,-2.1434188269279));
#26254=CARTESIAN_POINT('Ctrl Pts',(-41.6898193365417,3.99271145407791,-1.16273422749369));
#26255=CARTESIAN_POINT('Ctrl Pts',(-41.6832121542179,4.10850532121644,-0.64332860102408));
#26256=CARTESIAN_POINT('Ctrl Pts',(-41.6694431045306,4.13880671511246,0.431719161751283));
#26257=CARTESIAN_POINT('Ctrl Pts',(-41.6624066525318,4.044876135757,0.977284200391839));
#26258=CARTESIAN_POINT('Ctrl Pts',(-41.6493809475519,3.65700162885682,1.97974784987871));
#26259=CARTESIAN_POINT('Ctrl Pts',(-41.6437962991127,3.37459401737114,2.43005714560394));
#26260=CARTESIAN_POINT('Ctrl Pts',(-41.6309357144839,2.6511648782504,3.20490279380071));
#26261=CARTESIAN_POINT('Ctrl Pts',(-41.6240950523528,2.21501810087195,3.52047828305974));
#26262=CARTESIAN_POINT('Ctrl Pts',(-41.6102685834166,1.23516775348485,3.97344470167659));
#26263=CARTESIAN_POINT('Ctrl Pts',(-41.6034198208226,0.69881157589226,4.10189875001512));
#26264=CARTESIAN_POINT('Ctrl Pts',(-41.5910960941911,-0.368151649154125,
4.14150890791189));
#26265=CARTESIAN_POINT('Ctrl Pts',(-41.5852399688694,-0.888308013753419,
4.06184052114298));
#26266=CARTESIAN_POINT('Ctrl Pts',(-41.5719493419555,-1.88821115154311,
3.70692788444243));
#26267=CARTESIAN_POINT('Ctrl Pts',(-41.5649640886082,-2.35630439073406,
3.42848137615101));
#26268=CARTESIAN_POINT('Ctrl Pts',(-41.5512205553717,-3.16525635115029,
2.70135906194979));
#26269=CARTESIAN_POINT('Ctrl Pts',(-41.5448789620358,-3.49586139456939,
2.25723915262381));
#26270=CARTESIAN_POINT('Ctrl Pts',(-41.5326342043063,-3.9544771530286,1.28612950930069));
#26271=CARTESIAN_POINT('Ctrl Pts',(-41.5261040609182,-4.08604265353204,
0.772182183164868));
#26272=CARTESIAN_POINT('Ctrl Pts',(-41.5124134013752,-4.15034109753943,
-0.297938330209873));
#26273=CARTESIAN_POINT('Ctrl Pts',(-41.5053735373433,-4.07444377836835,
-0.844399243679091));
#26274=CARTESIAN_POINT('Ctrl Pts',(-41.4921889978187,-3.71957997578257,
-1.86040478998788));
#26275=CARTESIAN_POINT('Ctrl Pts',(-41.4865505274689,-3.45010848821036,
-2.32231169383177));
#26276=CARTESIAN_POINT('Ctrl Pts',(-41.4738145603255,-2.74996538392358,
-3.1202600661284));
#26277=CARTESIAN_POINT('Ctrl Pts',(-41.4670284180359,-2.32530046045201,
-3.44837711027349));
#26278=CARTESIAN_POINT('Ctrl Pts',(-41.4532046264246,-1.36189166545342,
-3.93182103888445));
#26279=CARTESIAN_POINT('Ctrl Pts',(-41.4463017518192,-0.829869995784418,
-4.07741206503004));
#26280=CARTESIAN_POINT('Ctrl Pts',(-41.4387871633191,-0.189989831523175,
-4.12172195295433));
#26281=CARTESIAN_POINT('Ctrl Pts',(-41.4376908908779,-0.0949462424977904,
-4.12499999999999));
#26282=CARTESIAN_POINT('Ctrl Pts',(-41.4366154631359,1.00826204764594E-14,
-4.12499999999999));
#26283=CARTESIAN_POINT('Origin',(-44.,0.,0.));
#26284=CARTESIAN_POINT('',(-41.1191154638315,-3.0705135232325E-8,-4.12499999999999));
#26285=CARTESIAN_POINT('',(-41.1984904632914,3.14162372061423E-8,-4.12499999999999));
#26286=CARTESIAN_POINT('',(-44.,-5.05166804648282E-16,-4.12499999999999));
#26287=CARTESIAN_POINT('Ctrl Pts',(-41.1984904636472,3.14203072240837E-8,
-4.12499999999999));
#26288=CARTESIAN_POINT('Ctrl Pts',(-41.2004042872906,-0.168965634416243,
-4.12500000128701));
#26289=CARTESIAN_POINT('Ctrl Pts',(-41.2023825656739,-0.338101978249229,
-4.114618703125));
#26290=CARTESIAN_POINT('Ctrl Pts',(-41.2110030427661,-1.05220486136019,
-4.02627570612251));
#26291=CARTESIAN_POINT('Ctrl Pts',(-41.2180295293847,-1.5789854227773,-3.85030260331271));
#26292=CARTESIAN_POINT('Ctrl Pts',(-41.2318603414182,-2.51421818099586,
-3.31270156035402));
#26293=CARTESIAN_POINT('Ctrl Pts',(-41.2385347595153,-2.91777039863962,
-2.96342838054045));
#26294=CARTESIAN_POINT('Ctrl Pts',(-41.2510423657805,-3.57618020949202,
-2.12490896476215));
#26295=CARTESIAN_POINT('Ctrl Pts',(-41.2569158946691,-3.82225694858102,
-1.6415416877236));
#26296=CARTESIAN_POINT('Ctrl Pts',(-41.27037385398,-4.11679795812124,-0.602102805487428));
#26297=CARTESIAN_POINT('Ctrl Pts',(-41.2774013732852,-4.16022530825056,
-0.0554709077489143));
#26298=CARTESIAN_POINT('Ctrl Pts',(-41.2909172897172,-4.0351898209026,1.00314057981436));
#26299=CARTESIAN_POINT('Ctrl Pts',(-41.2972413020317,-3.87567202277939,
1.50605216667389));
#26300=CARTESIAN_POINT('Ctrl Pts',(-41.3091708039741,-3.36630412025233,
2.44575960254218));
#26301=CARTESIAN_POINT('Ctrl Pts',(-41.3158899774543,-3.01337777792877,
2.86937050451361));
#26302=CARTESIAN_POINT('Ctrl Pts',(-41.3296788863341,-2.17037455234931,
3.54867430021675));
#26303=CARTESIAN_POINT('Ctrl Pts',(-41.3366091344405,-1.69078914481731,
3.80063805434704));
#26304=CARTESIAN_POINT('Ctrl Pts',(-41.3497088930555,-0.675441298380965,
4.10275667587154));
#26305=CARTESIAN_POINT('Ctrl Pts',(-41.3553517360618,-0.150664019239523,
4.15525340870424));
#26306=CARTESIAN_POINT('Ctrl Pts',(-41.3680534433334,0.919496695149706,
4.05889558137054));
#26307=CARTESIAN_POINT('Ctrl Pts',(-41.3750621471651,1.45359422294924,3.89963640912485));
#26308=CARTESIAN_POINT('Ctrl Pts',(-41.3889453632281,2.4086002008445,3.39052202916359));
#26309=CARTESIAN_POINT('Ctrl Pts',(-41.3956852034788,2.824189305568,3.05302401047762));
#26310=CARTESIAN_POINT('Ctrl Pts',(-41.408322946054,3.50624077004482,2.23735977487124));
#26311=CARTESIAN_POINT('Ctrl Pts',(-41.4140416444253,3.76561366420139,1.76625562075626));
#26312=CARTESIAN_POINT('Ctrl Pts',(-41.4273466055861,4.09451215588275,0.739950425480524));
#26313=CARTESIAN_POINT('Ctrl Pts',(-41.4343840485107,4.15634843276931,0.193187336624593));
#26314=CARTESIAN_POINT('Ctrl Pts',(-41.4480042183726,4.06567365410874,-0.872356044391565));
#26315=CARTESIAN_POINT('Ctrl Pts',(-41.4544700226359,3.92193758677376,-1.38170990687377));
#26316=CARTESIAN_POINT('Ctrl Pts',(-41.4665219163392,3.44167337160256,-2.33853208454178));
#26317=CARTESIAN_POINT('Ctrl Pts',(-41.4730195565733,3.10219191222297,-2.7731339278448));
#26318=CARTESIAN_POINT('Ctrl Pts',(-41.4867718677304,2.27962297532667,-3.47975578357437));
#26319=CARTESIAN_POINT('Ctrl Pts',(-41.4937364829231,1.80656753398599,-3.74722517231711));
#26320=CARTESIAN_POINT('Ctrl Pts',(-41.5059384302564,0.877091854307792,
-4.05469718261492));
#26321=CARTESIAN_POINT('Ctrl Pts',(-41.5110103044948,0.439683126898675,
-4.12499999999999));
#26322=CARTESIAN_POINT('Ctrl Pts',(-41.5159904640031,-1.18330754202892E-14,
-4.12499999999999));
#26323=CARTESIAN_POINT('Ctrl Pts',(-41.4366154631359,1.00826204764594E-14,
-4.12499999999999));
#26324=CARTESIAN_POINT('Ctrl Pts',(-41.4317940371804,0.425669024604756,
-4.12499999999999));
#26325=CARTESIAN_POINT('Ctrl Pts',(-41.4268949318863,0.849375791545828,
-4.05910724870507));
#26326=CARTESIAN_POINT('Ctrl Pts',(-41.4149033936746,1.76813330683894,-3.76543441969213));
#26327=CARTESIAN_POINT('Ctrl Pts',(-41.4079495348907,2.24342129297016,-3.50312015033128));
#26328=CARTESIAN_POINT('Ctrl Pts',(-41.3941837491158,3.07288942831861,-2.80555716233585));
#26329=CARTESIAN_POINT('Ctrl Pts',(-41.3875981767775,3.41688030312777,-2.37459638194406));
#26330=CARTESIAN_POINT('Ctrl Pts',(-41.375623100298,3.90691815915836,-1.42342466553835));
#26331=CARTESIAN_POINT('Ctrl Pts',(-41.3691866776663,4.05595320297728,-0.916177533959273));
#26332=CARTESIAN_POINT('Ctrl Pts',(-41.3555999968818,4.15815176059325,0.14715610915311));
#26333=CARTESIAN_POINT('Ctrl Pts',(-41.3485650216949,4.10247827203129,0.693941923109606));
#26334=CARTESIAN_POINT('Ctrl Pts',(-41.3352082450052,3.785032576777,1.72468868416642));
#26335=CARTESIAN_POINT('Ctrl Pts',(-41.3294439600945,3.53009840798865,2.19986935707565));
#26336=CARTESIAN_POINT('Ctrl Pts',(-41.3168495808063,2.85596491216151,3.02322492890188));
#26337=CARTESIAN_POINT('Ctrl Pts',(-41.3101310458571,2.44438625515306,3.36472789343333));
#26338=CARTESIAN_POINT('Ctrl Pts',(-41.2962639281764,1.49593664801328,3.88349997977635));
#26339=CARTESIAN_POINT('Ctrl Pts',(-41.2892484157969,0.964243672942856,
4.04841197387696));
#26340=CARTESIAN_POINT('Ctrl Pts',(-41.2764892467617,-0.104631011406712,
4.15672963094904));
#26341=CARTESIAN_POINT('Ctrl Pts',(-41.2708722798639,-0.630461211216935,
4.1099719745518));
#26342=CARTESIAN_POINT('Ctrl Pts',(-41.2578135827526,-1.64893728802458,
3.81889984176855));
#26343=CARTESIAN_POINT('Ctrl Pts',(-41.2508971823998,-2.13074152766268,
3.57252400847945));
#26344=CARTESIAN_POINT('Ctrl Pts',(-41.2370975291885,-2.98090443188783,
2.90309756948463));
#26345=CARTESIAN_POINT('Ctrl Pts',(-41.230353540608,-3.33859389179644,2.48345887136472));
#26346=CARTESIAN_POINT('Ctrl Pts',(-41.2183536245615,-3.85828119023053,
1.54990778949892));
#26347=CARTESIAN_POINT('Ctrl Pts',(-41.2121287394241,-4.02337456439361,
1.0492964816937));
#26348=CARTESIAN_POINT('Ctrl Pts',(-41.1986517713558,-4.1605053726292,-0.00669940082423867));
#26349=CARTESIAN_POINT('Ctrl Pts',(-41.1916295921606,-4.12357675364772,
-0.553141709230854));
#26350=CARTESIAN_POINT('Ctrl Pts',(-41.1781189185054,-3.84127647443778,
-1.59711978036542));
#26351=CARTESIAN_POINT('Ctrl Pts',(-41.1721774070469,-3.59992621745098,
-2.08487947020022));
#26352=CARTESIAN_POINT('Ctrl Pts',(-41.1597161953658,-2.94985948018453,
-2.93138640074789));
#26353=CARTESIAN_POINT('Ctrl Pts',(-41.1530661326808,-2.55059699927362,
-3.28468334129481));
#26354=CARTESIAN_POINT('Ctrl Pts',(-41.1392568744909,-1.62247801565102,
-3.83208457025847));
#26355=CARTESIAN_POINT('Ctrl Pts',(-41.13222591755,-1.09837547570754,-4.01383656740647));
#26356=CARTESIAN_POINT('Ctrl Pts',(-41.1233819784795,-0.370064243632087,
-4.11256198139676));
#26357=CARTESIAN_POINT('Ctrl Pts',(-41.1212103068118,-0.184947372187953,
-4.12499999862313));
#26358=CARTESIAN_POINT('Ctrl Pts',(-41.1191154634838,-3.07091125445469E-8,
-4.12499999999999));
#26359=CARTESIAN_POINT('Origin',(-44.,0.,0.));
#26360=CARTESIAN_POINT('',(-40.8016154631359,1.23927878701591E-15,-4.12499999999999));
#26361=CARTESIAN_POINT('',(-40.8809904640031,1.31047873626973E-14,-4.12499999999999));
#26362=CARTESIAN_POINT('',(-44.,-5.05166804648282E-16,-4.12499999999999));
#26363=CARTESIAN_POINT('Ctrl Pts',(-40.8809904640031,3.10168557504653E-14,
-4.12499999999999));
#26364=CARTESIAN_POINT('Ctrl Pts',(-40.8839470138832,-0.26102479127236,
-4.12499999999999));
#26365=CARTESIAN_POINT('Ctrl Pts',(-40.8870529019846,-0.522060729148633,
-4.10022430546627));
#26366=CARTESIAN_POINT('Ctrl Pts',(-40.8969646800572,-1.31590810541924,
-3.94744660305077));
#26367=CARTESIAN_POINT('Ctrl Pts',(-40.9040045032918,-1.82645051981365,
-3.73871952743978));
#26368=CARTESIAN_POINT('Ctrl Pts',(-40.9176885650803,-2.71938071075019,
-3.1459258679918));
#26369=CARTESIAN_POINT('Ctrl Pts',(-40.9242125192711,-3.09770419502207,
-2.77418791269944));
#26370=CARTESIAN_POINT('Ctrl Pts',(-40.9364465459559,-3.70752266479565,
-1.88970761857416));
#26371=CARTESIAN_POINT('Ctrl Pts',(-40.9428113492738,-3.92574569379075,
-1.38030921310186));
#26372=CARTESIAN_POINT('Ctrl Pts',(-40.9565658541248,-4.14814848331695,
-0.315220576048532));
#26373=CARTESIAN_POINT('Ctrl Pts',(-40.963548778103,-4.15378670615725,0.229252499479745));
#26374=CARTESIAN_POINT('Ctrl Pts',(-40.9768299884806,-3.9584895041917,1.27201044419376));
#26375=CARTESIAN_POINT('Ctrl Pts',(-40.9826718505753,-3.76611658540577,
1.76181953416122));
#26376=CARTESIAN_POINT('Ctrl Pts',(-40.9950114172715,-3.19594937715089,
2.66454953000424));
#26377=CARTESIAN_POINT('Ctrl Pts',(-41.001864890921,-2.8154718999071,3.06382536801303));
#26378=CARTESIAN_POINT('Ctrl Pts',(-41.0156916787708,-1.93173850362775,
3.68351937831143));
#26379=CARTESIAN_POINT('Ctrl Pts',(-41.0225281091007,-1.43992902586759,
3.90211964688776));
#26380=CARTESIAN_POINT('Ctrl Pts',(-41.0353785939384,-0.406484012832493,
4.13860780742009));
#26381=CARTESIAN_POINT('Ctrl Pts',(-41.0409655408276,0.124983314558916,
4.15664324157981));
#26382=CARTESIAN_POINT('Ctrl Pts',(-41.0540043698413,1.18670756229525,3.98844181504285));
#26383=CARTESIAN_POINT('Ctrl Pts',(-41.0610413736391,1.70549307778222,3.79568590729839));
#26384=CARTESIAN_POINT('Ctrl Pts',(-41.0748045405807,2.61965908259185,3.22969609932009));
#26385=CARTESIAN_POINT('Ctrl Pts',(-41.0814056757731,3.01056525603536,2.86880732798728));
#26386=CARTESIAN_POINT('Ctrl Pts',(-41.0937764079445,3.64448434837413,2.00695463922163));
#26387=CARTESIAN_POINT('Ctrl Pts',(-41.099868960675,3.87662568440571,1.51060067487246));
#26388=CARTESIAN_POINT('Ctrl Pts',(-41.1134796197322,4.13506274571464,0.457990393297178));
#26389=CARTESIAN_POINT('Ctrl Pts',(-41.1204887333393,4.15942031041744,-0.0878717865673329));
#26390=CARTESIAN_POINT('Ctrl Pts',(-41.1338886885907,3.99891612317659,-1.13867686484691));
#26391=CARTESIAN_POINT('Ctrl Pts',(-41.13994064032,3.82295917353972,-1.63489610003659));
#26392=CARTESIAN_POINT('Ctrl Pts',(-41.1520768794015,3.28315673221665,-2.55630976250079));
#26393=CARTESIAN_POINT('Ctrl Pts',(-41.1588668964708,2.91628103728796,-2.96801834399691));
#26394=CARTESIAN_POINT('Ctrl Pts',(-41.1726824579823,2.05244569098672,-3.61790446180448));
#26395=CARTESIAN_POINT('Ctrl Pts',(-41.1795694303592,1.56648346783269,-3.85329718460974));
#26396=CARTESIAN_POINT('Ctrl Pts',(-41.190468584663,0.706031521498386,-4.07958539149015));
#26397=CARTESIAN_POINT('Ctrl Pts',(-41.1944877121763,0.353390778668214,
-4.1249999973082));
#26398=CARTESIAN_POINT('Ctrl Pts',(-41.1984904636472,3.1420303382781E-8,
-4.12499999999999));
#26399=CARTESIAN_POINT('Ctrl Pts',(-41.1191154634838,-3.07091139260437E-8,
-4.12499999999999));
#26400=CARTESIAN_POINT('Ctrl Pts',(-41.1152860126284,0.338090529834655,
-4.12500000251695));
#26401=CARTESIAN_POINT('Ctrl Pts',(-41.1114506786048,0.675611576268281,
-4.08343304902581));
#26402=CARTESIAN_POINT('Ctrl Pts',(-41.1007837261389,1.52310611262671,-3.87056625707979));
#26403=CARTESIAN_POINT('Ctrl Pts',(-41.0939133549729,2.01114439427458,-3.64093801160786));
#26404=CARTESIAN_POINT('Ctrl Pts',(-41.0800921712788,2.88194622251291,-3.00137355503281));
#26405=CARTESIAN_POINT('Ctrl Pts',(-41.0732794357799,3.25355108826573,-2.5938912779187));
#26406=CARTESIAN_POINT('Ctrl Pts',(-41.0610727172601,3.80382762960107,-1.67887193692206));
#26407=CARTESIAN_POINT('Ctrl Pts',(-41.0551001677632,3.98544290848857,-1.18489296223169));
#26408=CARTESIAN_POINT('Ctrl Pts',(-41.0417408498085,4.15801392901122,-0.13683622103637));
#26409=CARTESIAN_POINT('Ctrl Pts',(-41.0347399039998,4.14014941659439,0.408615610718514));
#26410=CARTESIAN_POINT('Ctrl Pts',(-41.0210786526762,3.89414024647464,1.46560609433591));
#26411=CARTESIAN_POINT('Ctrl Pts',(-41.0148980575338,3.66679578896948,1.96645071832313));
#26412=CARTESIAN_POINT('Ctrl Pts',(-41.0025744628787,3.04122646956046,2.83618016236111));
#26413=CARTESIAN_POINT('Ctrl Pts',(-40.9959995199361,2.65466604187339,3.20089303689757));
#26414=CARTESIAN_POINT('Ctrl Pts',(-40.9822623901042,1.74780447029673,3.77629718990782));
#26415=CARTESIAN_POINT('Ctrl Pts',(-40.9752235810873,1.23183458420386,3.97464827148568));
#26416=CARTESIAN_POINT('Ctrl Pts',(-40.9621292566798,0.171727153597128,
4.15510514463831));
#26417=CARTESIAN_POINT('Ctrl Pts',(-40.9565283722576,-0.360963948783399,
4.14295711179001));
#26418=CARTESIAN_POINT('Ctrl Pts',(-40.9437209756471,-1.39733836990323,
3.91749539509072));
#26419=CARTESIAN_POINT('Ctrl Pts',(-40.9369029772592,-1.89097413188998,
3.7045291876586));
#26420=CARTESIAN_POINT('Ctrl Pts',(-40.9230759075655,-2.78111561604286,
3.09504880154495));
#26421=CARTESIAN_POINT('Ctrl Pts',(-40.9162029883302,-3.1660382402763,2.70002618019827));
#26422=CARTESIAN_POINT('Ctrl Pts',(-40.9037965342527,-3.74629750031841,
1.80360750350104));
#26423=CARTESIAN_POINT('Ctrl Pts',(-40.8980109075797,-3.94413844250431,
1.31587350265686));
#26424=CARTESIAN_POINT('Ctrl Pts',(-40.8847697694036,-4.15087445447382,
0.27584174848787));
#26425=CARTESIAN_POINT('Ctrl Pts',(-40.8777972220417,-4.15138561118553,
-0.268036689214984));
#26426=CARTESIAN_POINT('Ctrl Pts',(-40.8639968365375,-3.94096336839514,
-1.3371223995839));
#26427=CARTESIAN_POINT('Ctrl Pts',(-40.857530323586,-3.7273776994595,-1.8508722670883));
#26428=CARTESIAN_POINT('Ctrl Pts',(-40.8453417721317,-3.12549978411905,
-2.74273570037126));
#26429=CARTESIAN_POINT('Ctrl Pts',(-40.8388442759054,-2.75134560113339,
-3.11792179483804));
#26430=CARTESIAN_POINT('Ctrl Pts',(-40.8251888704923,-1.86550885922186,
-3.71929808341301));
#26431=CARTESIAN_POINT('Ctrl Pts',(-40.8181496958091,-1.35775745373826,
-3.93316659552598));
#26432=CARTESIAN_POINT('Ctrl Pts',(-40.808029911448,-0.551601820026865,
-4.09733394871241));
#26433=CARTESIAN_POINT('Ctrl Pts',(-40.8047397042343,-0.275829738591203,
-4.12499999999999));
#26434=CARTESIAN_POINT('Ctrl Pts',(-40.8016154631359,-9.0205620750794E-15,
-4.12499999999999));
#26435=CARTESIAN_POINT('Origin',(-44.,0.,0.));
#26436=CARTESIAN_POINT('',(-40.4841154631359,8.00470034332546E-15,-4.12499999999999));
#26437=CARTESIAN_POINT('',(-40.5634904640031,-9.48131229452075E-15,-4.12499999999999));
#26438=CARTESIAN_POINT('',(-44.,-5.05166804648282E-16,-4.12499999999999));
#26439=CARTESIAN_POINT('Ctrl Pts',(-40.5634904640031,-1.4363510381088E-14,
-4.12499999999999));
#26440=CARTESIAN_POINT('Ctrl Pts',(-40.5675734140323,-0.360471232468091,
-4.12499999999999));
#26441=CARTESIAN_POINT('Ctrl Pts',(-40.571932143759,-0.720165512036405,
-4.07774730593135));
#26442=CARTESIAN_POINT('Ctrl Pts',(-40.5832363854935,-1.59349134286567,
-3.84323713483626));
#26443=CARTESIAN_POINT('Ctrl Pts',(-40.5902571703085,-2.08437704877094,
-3.60070237538558));
#26444=CARTESIAN_POINT('Ctrl Pts',(-40.6037249008704,-2.92837251785335,
-2.95179630856995));
#26445=CARTESIAN_POINT('Ctrl Pts',(-40.6099274472567,-3.27824553450907,
-2.5576465443238));
#26446=CARTESIAN_POINT('Ctrl Pts',(-40.6219439142245,-3.82440199459883,
-1.63943106145909));
#26447=CARTESIAN_POINT('Ctrl Pts',(-40.6286936343242,-4.007596999902,-1.11934837125817));
#26448=CARTESIAN_POINT('Ctrl Pts',(-40.6424955661354,-4.1593901361805,-0.048094675003366));
#26449=CARTESIAN_POINT('Ctrl Pts',(-40.6494085791874,-4.13045370680168,
0.492132702753004));
#26450=CARTESIAN_POINT('Ctrl Pts',(-40.6624575231156,-3.87066496912996,
1.51902589539787));
#26451=CARTESIAN_POINT('Ctrl Pts',(-40.6680693413401,-3.64693990695748,
1.99732679628217));
#26452=CARTESIAN_POINT('Ctrl Pts',(-40.680842044632,-3.0163991495834,2.86715464410791));
#26453=CARTESIAN_POINT('Ctrl Pts',(-40.6878590472127,-2.60686785534687,
3.24399026501724));
#26454=CARTESIAN_POINT('Ctrl Pts',(-40.7017221237258,-1.68218512502133,
3.80348981623548));
#26455=CARTESIAN_POINT('Ctrl Pts',(-40.7084355068985,-1.18030743090806,
3.98787695473004));
#26456=CARTESIAN_POINT('Ctrl Pts',(-40.7210195525044,-0.129556763979266,
4.15747624818416));
#26457=CARTESIAN_POINT('Ctrl Pts',(-40.7267955976369,0.409743228067629,
4.13926407299677));
#26458=CARTESIAN_POINT('Ctrl Pts',(-40.7401645996931,1.46066303086723,3.89591931502526));
#26459=CARTESIAN_POINT('Ctrl Pts',(-40.7471988621716,1.96129409504847,3.66947502882011));
#26460=CARTESIAN_POINT('Ctrl Pts',(-40.7607773519379,2.82923062666211,3.047204693113));
#26461=CARTESIAN_POINT('Ctrl Pts',(-40.7672066864071,3.19293317205768,2.66367975186589));
#26462=CARTESIAN_POINT('Ctrl Pts',(-40.7791633166215,3.7693195703258,1.76238278909522));
#26463=CARTESIAN_POINT('Ctrl Pts',(-40.7857705616497,3.96925798059591,1.24850966615598));
#26464=CARTESIAN_POINT('Ctrl Pts',(-40.799539335584,4.15594352225663,0.18106076295438));
#26465=CARTESIAN_POINT('Ctrl Pts',(-40.8064905315325,4.14414474838805,-0.361546430985013));
#26466=CARTESIAN_POINT('Ctrl Pts',(-40.8196567319039,3.91638435717499,-1.39646720353316));
#26467=CARTESIAN_POINT('Ctrl Pts',(-40.8253561135646,3.70839290177736,-1.88042683332904));
#26468=CARTESIAN_POINT('Ctrl Pts',(-40.8378854635978,3.10944612457397,-2.76501760465572));
#26469=CARTESIAN_POINT('Ctrl Pts',(-40.8447921762378,2.71639790136549,-3.15200766330559));
#26470=CARTESIAN_POINT('Ctrl Pts',(-40.8586151755949,1.81467031067166,-3.74234764402162));
#26471=CARTESIAN_POINT('Ctrl Pts',(-40.8653968890452,1.31781029025714,-3.94481633328329));
#26472=CARTESIAN_POINT('Ctrl Pts',(-40.8749800234564,0.533357374710669,
-4.09913783379567));
#26473=CARTESIAN_POINT('Ctrl Pts',(-40.877969800176,0.266685216526378,-4.12499999999999));
#26474=CARTESIAN_POINT('Ctrl Pts',(-40.8809904640031,3.17182435821952E-14,
-4.12499999999999));
#26475=CARTESIAN_POINT('Ctrl Pts',(-40.8016154631359,-1.28833483865871E-14,
-4.12499999999999));
#26476=CARTESIAN_POINT('Ctrl Pts',(-40.7987491667761,0.253056582631218,
-4.12499999999999));
#26477=CARTESIAN_POINT('Ctrl Pts',(-40.7959184081503,0.506160509587679,
-4.10171373271893));
#26478=CARTESIAN_POINT('Ctrl Pts',(-40.7865416494958,1.27813394217847,-3.95777939416467));
#26479=CARTESIAN_POINT('Ctrl Pts',(-40.7797789333525,1.77651344586574,-3.76053694882057));
#26480=CARTESIAN_POINT('Ctrl Pts',(-40.7659601690815,2.68383921778971,-3.17977892504124));
#26481=CARTESIAN_POINT('Ctrl Pts',(-40.7590378055941,3.08085732675141,-2.79683972378313));
#26482=CARTESIAN_POINT('Ctrl Pts',(-40.7464480969967,3.68905485419697,-1.91817431678888));
#26483=CARTESIAN_POINT('Ctrl Pts',(-40.7407828262988,3.90208612855456,-1.43605207520613));
#26484=CARTESIAN_POINT('Ctrl Pts',(-40.7276540591317,4.14018118830279,-0.403690208174394));
#26485=CARTESIAN_POINT('Ctrl Pts',(-40.7207144391096,4.15751878480496,0.138207480308497));
#26486=CARTESIAN_POINT('Ctrl Pts',(-40.7069342644054,3.98208570997053,1.20693859145346));
#26487=CARTESIAN_POINT('Ctrl Pts',(-40.7002333014212,3.78755871206735,1.72282249150634));
#26488=CARTESIAN_POINT('Ctrl Pts',(-40.6883542753676,3.22096473485822,2.62960385192518));
#26489=CARTESIAN_POINT('Ctrl Pts',(-40.6819551684805,2.86175752493203,3.01658708980989));
#26490=CARTESIAN_POINT('Ctrl Pts',(-40.668411685601,2.00155042900569,3.64758170969355));
#26491=CARTESIAN_POINT('Ctrl Pts',(-40.6613809279315,1.50403158161056,3.87929727322067));
#26492=CARTESIAN_POINT('Ctrl Pts',(-40.6479611935944,0.455056611180836,
4.13472350026447));
#26493=CARTESIAN_POINT('Ctrl Pts',(-40.6421321536017,-0.0855688602521068,
4.15880863776603));
#26494=CARTESIAN_POINT('Ctrl Pts',(-40.6295914262721,-1.1389622030828,3.99981076167824));
#26495=CARTESIAN_POINT('Ctrl Pts',(-40.6228999424275,-1.64221384336218,
3.82084385528187));
#26496=CARTESIAN_POINT('Ctrl Pts',(-40.609054644058,-2.57177890670439,3.27177288984792));
#26497=CARTESIAN_POINT('Ctrl Pts',(-40.6020319376635,-2.98488904384758,
2.89982556624254));
#26498=CARTESIAN_POINT('Ctrl Pts',(-40.5892031578238,-3.62498922247056,
2.03704695742646));
#26499=CARTESIAN_POINT('Ctrl Pts',(-40.5836087707956,-3.85415098979506,
1.56065010585271));
#26500=CARTESIAN_POINT('Ctrl Pts',(-40.5706005753391,-4.12484416838145,
0.536554513603813));
#26501=CARTESIAN_POINT('Ctrl Pts',(-40.5637021117861,-4.15959364278306,
-0.00274099528344514));
#26502=CARTESIAN_POINT('Ctrl Pts',(-40.5498917708271,-4.01970620139322,
-1.07506636337484));
#26503=CARTESIAN_POINT('Ctrl Pts',(-40.5431187668493,-3.84224905068353,
-1.59716557269067));
#26504=CARTESIAN_POINT('Ctrl Pts',(-40.5310338571766,-3.30639681266052,
-2.5210794364958));
#26505=CARTESIAN_POINT('Ctrl Pts',(-40.5249197608055,-2.96116162576673,
-2.91884190336009));
#26506=CARTESIAN_POINT('Ctrl Pts',(-40.5114905610946,-2.1252829111401,-3.57661556325932));
#26507=CARTESIAN_POINT('Ctrl Pts',(-40.5044761054092,-1.63779006275009,
-3.82448044806031));
#26508=CARTESIAN_POINT('Ctrl Pts',(-40.4929472200596,-0.752298941107392,
-4.07341167294306));
#26509=CARTESIAN_POINT('Ctrl Pts',(-40.4883815963868,-0.376643921628896,
-4.12499999999999));
#26510=CARTESIAN_POINT('Ctrl Pts',(-40.4841154631359,3.19883008970123E-14,
-4.12499999999999));
#26511=CARTESIAN_POINT('Origin',(-44.,0.,0.));
#26512=CARTESIAN_POINT('',(-40.1666154631359,-6.3588100377625E-15,-4.12499999999999));
#26513=CARTESIAN_POINT('',(-40.2459904640031,-1.4997732948127E-14,-4.12499999999999));
#26514=CARTESIAN_POINT('',(-44.,-5.05166804648282E-16,-4.12499999999999));
#26515=CARTESIAN_POINT('Ctrl Pts',(-40.2459904640031,-1.08246744900953E-14,
-4.12499999999999));
#26516=CARTESIAN_POINT('Ctrl Pts',(-40.2511645331132,-0.456802815521309,
-4.12499999999999));
#26517=CARTESIAN_POINT('Ctrl Pts',(-40.2567671388541,-0.911090653036704,
-4.04911424251985));
#26518=CARTESIAN_POINT('Ctrl Pts',(-40.2693950955372,-1.85330635565894,
-3.7243726598499));
#26519=CARTESIAN_POINT('Ctrl Pts',(-40.2763651340528,-2.32323014163459,
-3.45084036187277));
#26520=CARTESIAN_POINT('Ctrl Pts',(-40.2895969905501,-3.1186938864387,-2.7498247794128));
#26521=CARTESIAN_POINT('Ctrl Pts',(-40.295370610222,-3.44112113451425,-2.33376677506535));
#26522=CARTESIAN_POINT('Ctrl Pts',(-40.3077924387886,-3.92488219124724,
-1.38175408190277));
#26523=CARTESIAN_POINT('Ctrl Pts',(-40.3146697241653,-4.07315395093914,
-0.850501718841946));
#26524=CARTESIAN_POINT('Ctrl Pts',(-40.3284966127207,-4.15312669191325,
0.225206633704283));
#26525=CARTESIAN_POINT('Ctrl Pts',(-40.3353102446371,-4.08940826849617,
0.758896869890493));
#26526=CARTESIAN_POINT('Ctrl Pts',(-40.3481076346137,-3.76393320782021,
1.76846260293689));
#26527=CARTESIAN_POINT('Ctrl Pts',(-40.3537127053316,-3.5067823671733,2.23542637049589));
#26528=CARTESIAN_POINT('Ctrl Pts',(-40.3668198019382,-2.81818007320255,
3.0615266230001));
#26529=CARTESIAN_POINT('Ctrl Pts',(-40.3738589036421,-2.38763015013398,
3.40797625552582));
#26530=CARTESIAN_POINT('Ctrl Pts',(-40.3875897705407,-1.43485943880383,
3.90307719940798));
#26531=CARTESIAN_POINT('Ctrl Pts',(-40.3941585404323,-0.925473555718519,
4.05417566477752));
#26532=CARTESIAN_POINT('Ctrl Pts',(-40.4064711435521,0.141129194611049,
4.15847629606445));
#26533=CARTESIAN_POINT('Ctrl Pts',(-40.4126731645028,0.688894074985228,
4.10344704284241));
#26534=CARTESIAN_POINT('Ctrl Pts',(-40.4263460636897,1.72670495377073,3.78498780607248));
#26535=CARTESIAN_POINT('Ctrl Pts',(-40.4333449731268,2.20716624280072,3.52647983676792));
#26536=CARTESIAN_POINT('Ctrl Pts',(-40.446694767345,3.02656439153977,2.85089551558366));
#26537=CARTESIAN_POINT('Ctrl Pts',(-40.452649855385,3.3624468926465,2.4457386866896));
#26538=CARTESIAN_POINT('Ctrl Pts',(-40.4648729533427,3.87722024233396,1.51031000812043));
#26539=CARTESIAN_POINT('Ctrl Pts',(-40.4716908604004,4.04289787582651,0.984296996577499));
#26540=CARTESIAN_POINT('Ctrl Pts',(-40.4855130908483,4.15847552344624,-0.0898046715788642));
#26541=CARTESIAN_POINT('Ctrl Pts',(-40.4923794658442,4.11191518262026,-0.627009708846587));
#26542=CARTESIAN_POINT('Ctrl Pts',(-40.5053033001154,3.81898505439463,-1.64530163712721));
#26543=CARTESIAN_POINT('Ctrl Pts',(-40.5108820741256,3.57860195755648,-2.11784602213624));
#26544=CARTESIAN_POINT('Ctrl Pts',(-40.523824578453,2.91890677962931,-2.96599529937724));
#26545=CARTESIAN_POINT('Ctrl Pts',(-40.5308564517633,2.49860365386708,-3.32777991648706));
#26546=CARTESIAN_POINT('Ctrl Pts',(-40.544660418758,1.55934370916937,-3.85525585600394));
#26547=CARTESIAN_POINT('Ctrl Pts',(-40.5513046650687,1.05344357974458,-4.02303550703667));
#26548=CARTESIAN_POINT('Ctrl Pts',(-40.5595335155396,0.353662903039793,
-4.11364157625598));
#26549=CARTESIAN_POINT('Ctrl Pts',(-40.5614886034933,0.176738172163106,
-4.12499999999999));
#26550=CARTESIAN_POINT('Ctrl Pts',(-40.5634904640031,-1.23582119034381E-14,
-4.12499999999999));
#26551=CARTESIAN_POINT('Ctrl Pts',(-40.4841154631359,3.13681525934293E-14,
-4.12499999999999));
#26552=CARTESIAN_POINT('Ctrl Pts',(-40.4822753706969,0.162456161504383,
-4.12499999999999));
#26553=CARTESIAN_POINT('Ctrl Pts',(-40.4804812668311,0.325096198638992,
-4.11540312943268));
#26554=CARTESIAN_POINT('Ctrl Pts',(-40.4724651726939,1.01097481237393,-4.03384622077745));
#26555=CARTESIAN_POINT('Ctrl Pts',(-40.4658453438792,1.51809459276297,-3.87161030816205));
#26556=CARTESIAN_POINT('Ctrl Pts',(-40.4520641552773,2.46196947749767,-3.35487058828514));
#26557=CARTESIAN_POINT('Ctrl Pts',(-40.4450290293083,2.88574115794718,-2.99815834290086));
#26558=CARTESIAN_POINT('Ctrl Pts',(-40.4320311675825,3.55508263011756,-2.15730311961309));
#26559=CARTESIAN_POINT('Ctrl Pts',(-40.4264501489989,3.80103124624296,-1.68663302019211));
#26560=CARTESIAN_POINT('Ctrl Pts',(-40.41356824869,4.10485447069414,-0.671231557054981));
#26561=CARTESIAN_POINT('Ctrl Pts',(-40.4067187680204,4.15717619845452,-0.135143089765433));
#26562=CARTESIAN_POINT('Ctrl Pts',(-40.3928932925976,4.05351566546605,0.939627842130299));
#26563=CARTESIAN_POINT('Ctrl Pts',(-40.3860546662005,3.8936436306417,1.46745970374505));
#26564=CARTESIAN_POINT('Ctrl Pts',(-40.3737645744268,3.38922878719453,2.40847564516003));
#26565=CARTESIAN_POINT('Ctrl Pts',(-40.3678769712427,3.05787925922361,2.81726992195831));
#26566=CARTESIAN_POINT('Ctrl Pts',(-40.3545664420887,2.24651754008161,3.50144885572143));
#26567=CARTESIAN_POINT('Ctrl Pts',(-40.3475764048178,1.76955239567787,3.76505895019985));
#26568=CARTESIAN_POINT('Ctrl Pts',(-40.3338563021928,0.734137805202703,
4.09586277936751));
#26569=CARTESIAN_POINT('Ctrl Pts',(-40.3275628767339,0.184939966494483,
4.15702242121256));
#26570=CARTESIAN_POINT('Ctrl Pts',(-40.3152953798184,-0.884140561094941,
4.06332232400762));
#26571=CARTESIAN_POINT('Ctrl Pts',(-40.3087521921069,-1.39453225494303,
3.91759670981335));
#26572=CARTESIAN_POINT('Ctrl Pts',(-40.2950477641159,-2.35141623776284,
3.43296762105789));
#26573=CARTESIAN_POINT('Ctrl Pts',(-40.2880079578197,-2.78514593313154,
3.09150304024689));
#26574=CARTESIAN_POINT('Ctrl Pts',(-40.2748491081645,-3.48298625464293,
2.27257368934654));
#26575=CARTESIAN_POINT('Ctrl Pts',(-40.2692232582875,-3.74555545626104,
1.80737321559898));
#26576=CARTESIAN_POINT('Ctrl Pts',(-40.2564667705712,-4.0813718577666,0.800636742382464));
#26577=CARTESIAN_POINT('Ctrl Pts',(-40.2496713147319,-4.15050504243521,
0.26817515751442));
#26578=CARTESIAN_POINT('Ctrl Pts',(-40.2358461129982,-4.08184039453985,
-0.807796509791499));
#26579=CARTESIAN_POINT('Ctrl Pts',(-40.2289515579117,-3.93913465550836,
-1.3405902846371));
#26580=CARTESIAN_POINT('Ctrl Pts',(-40.2164675004409,-3.46526878917106,
-2.29780239688099));
#26581=CARTESIAN_POINT('Ctrl Pts',(-40.2107389342126,-3.14706448761942,
-2.71734678090657));
#26582=CARTESIAN_POINT('Ctrl Pts',(-40.1975449173483,-2.35915715275628,
-3.42629087401622));
#26583=CARTESIAN_POINT('Ctrl Pts',(-40.1905855070596,-1.8926366192759,-3.70445900981677));
#26584=CARTESIAN_POINT('Ctrl Pts',(-40.1777562548584,-0.940557438244165,
-4.0440739233157));
#26585=CARTESIAN_POINT('Ctrl Pts',(-40.1719586032874,-0.471729583234032,
-4.12499999999999));
#26586=CARTESIAN_POINT('Ctrl Pts',(-40.1666154631359,-1.2490009027033E-14,
-4.12499999999999));
#26587=CARTESIAN_POINT('Origin',(-44.,0.,0.));
#26588=CARTESIAN_POINT('',(-39.8491154631359,1.54314928943905E-14,-4.12499999999999));
#26589=CARTESIAN_POINT('',(-39.9284904639595,1.92328552709179E-9,-4.12499999999999));
#26590=CARTESIAN_POINT('',(-44.,-5.05166804648282E-16,-4.12499999999999));
#26591=CARTESIAN_POINT('Ctrl Pts',(-39.9284904639595,3.84657155935038E-9,
-4.12499999999999));
#26592=CARTESIAN_POINT('Ctrl Pts',(-39.9285613255899,-0.00625615385321784,
-4.12500000000582));
#26593=CARTESIAN_POINT('Ctrl Pts',(-39.9286322803852,-0.0125129692164882,
-4.12498576746479));
#26594=CARTESIAN_POINT('Ctrl Pts',(-39.9349035628237,-0.564849025000654,
-4.1224723921527));
#26595=CARTESIAN_POINT('Ctrl Pts',(-39.941689948868,-1.10503267883579,-4.01157400752992));
#26596=CARTESIAN_POINT('Ctrl Pts',(-39.9555044655837,-2.10060887504081,
-3.59016819890216));
#26597=CARTESIAN_POINT('Ctrl Pts',(-39.9623939550971,-2.54805930694276,
-3.28774431673863));
#26598=CARTESIAN_POINT('Ctrl Pts',(-39.9753778551158,-3.29493450649213,
-2.53651856164694));
#26599=CARTESIAN_POINT('Ctrl Pts',(-39.9809649441868,-3.59033631924146,
-2.09761859456588));
#26600=CARTESIAN_POINT('Ctrl Pts',(-39.9938268014861,-4.01099550328834,
-1.1090799748115));
#26601=CARTESIAN_POINT('Ctrl Pts',(-40.0008525107595,-4.12297601485987,
-0.564983189194966));
#26602=CARTESIAN_POINT('Ctrl Pts',(-40.0146865276618,-4.12689303188455,
0.5139371007478));
#26603=CARTESIAN_POINT('Ctrl Pts',(-40.0213646683409,-4.02706797150972,
1.03831985518209));
#26604=CARTESIAN_POINT('Ctrl Pts',(-40.0338794544559,-3.63181818055359,
2.0282789975544));
#26605=CARTESIAN_POINT('Ctrl Pts',(-40.0397430506145,-3.33720204469592,
2.48336578946497));
#26606=CARTESIAN_POINT('Ctrl Pts',(-40.0531927654037,-2.58585361099515,
3.25945141792043));
#26607=CARTESIAN_POINT('Ctrl Pts',(-40.0602210275196,-2.13465491468969,
3.57126156886965));
#26608=CARTESIAN_POINT('Ctrl Pts',(-40.073742936908,-1.15594403833876,3.99411127763624));
#26609=CARTESIAN_POINT('Ctrl Pts',(-40.0800829220566,-0.640771741663391,
4.10834777384782));
#26610=CARTESIAN_POINT('Ctrl Pts',(-40.0920014966045,0.427745727565198,
4.13893364113017));
#26611=CARTESIAN_POINT('Ctrl Pts',(-40.098716757312,0.971223994379406,4.04604143043629));
#26612=CARTESIAN_POINT('Ctrl Pts',(-40.1125038478542,1.9817777368465,3.65735823047392));
#26613=CARTESIAN_POINT('Ctrl Pts',(-40.1194361638857,2.44034969934498,3.36873983532249));
#26614=CARTESIAN_POINT('Ctrl Pts',(-40.132542232477,3.21090076698186,2.64175660037354));
#26615=CARTESIAN_POINT('Ctrl Pts',(-40.1381896593882,3.51943910808138,2.21411543790356));
#26616=CARTESIAN_POINT('Ctrl Pts',(-40.1508156422579,3.97037755423067,1.24503246284474));
#26617=CARTESIAN_POINT('Ctrl Pts',(-40.1577471034709,4.10017612521246,0.70890927187637));
#26618=CARTESIAN_POINT('Ctrl Pts',(-40.1715625963995,4.14275938969906,-0.367215887972643));
#26619=CARTESIAN_POINT('Ctrl Pts',(-40.1783135140328,4.06120060776941,-0.896637392098473));
#26620=CARTESIAN_POINT('Ctrl Pts',(-40.1909742296231,3.70150240323432,-1.89673758441462));
#26621=CARTESIAN_POINT('Ctrl Pts',(-40.1966712706875,3.42624545922335,-2.35787560203382));
#26622=CARTESIAN_POINT('Ctrl Pts',(-40.2099484456965,2.7069837021752,-3.15992951396612));
#26623=CARTESIAN_POINT('Ctrl Pts',(-40.21698685119,2.26606326514222,-3.4896804402072));
#26624=CARTESIAN_POINT('Ctrl Pts',(-40.2306241797491,1.30003232585709,-3.94980080559581));
#26625=CARTESIAN_POINT('Ctrl Pts',(-40.2371053097944,0.787513969953535,
-4.08299417523486));
#26626=CARTESIAN_POINT('Ctrl Pts',(-40.2440258670844,0.175867960167723,
-4.12219123871433));
#26627=CARTESIAN_POINT('Ctrl Pts',(-40.2449949899983,0.0878873703636625,
-4.12499999999999));
#26628=CARTESIAN_POINT('Ctrl Pts',(-40.2459904640031,-1.23582119034381E-14,
-4.12499999999999));
#26629=CARTESIAN_POINT('Ctrl Pts',(-40.1666154631359,-1.28833483865871E-14,
-4.12499999999999));
#26630=CARTESIAN_POINT('Ctrl Pts',(-40.1657875078361,0.0730976537079367,
-4.12499999999999));
#26631=CARTESIAN_POINT('Ctrl Pts',(-40.1649788014734,0.146265079272092,
-4.1230570124755));
#26632=CARTESIAN_POINT('Ctrl Pts',(-40.1582718697332,0.742907530787551,
-4.09127421296842));
#26633=CARTESIAN_POINT('Ctrl Pts',(-40.1518204403058,1.25630263379554,-3.96385298436616));
#26634=CARTESIAN_POINT('Ctrl Pts',(-40.1382165597341,2.22633704610043,-3.51505981705709));
#26635=CARTESIAN_POINT('Ctrl Pts',(-40.1311802244293,2.67046358955764,-3.19074426475465));
#26636=CARTESIAN_POINT('Ctrl Pts',(-40.1178496794716,3.39953551237553,-2.39653901600989));
#26637=CARTESIAN_POINT('Ctrl Pts',(-40.1121093274993,3.68066420103062,-1.93725311097702));
#26638=CARTESIAN_POINT('Ctrl Pts',(-40.0994929087377,4.05125765893966,-0.940227612697416));
#26639=CARTESIAN_POINT('Ctrl Pts',(-40.0927634815047,4.13844542904659,-0.412285797036978));
#26640=CARTESIAN_POINT('Ctrl Pts',(-40.0788880069208,4.10758931019005,0.668927469168811));
#26641=CARTESIAN_POINT('Ctrl Pts',(-40.0718758421793,3.98146853579977,1.21147398876256));
#26642=CARTESIAN_POINT('Ctrl Pts',(-40.0591457428114,3.5352567600302,2.18884313792248));
#26643=CARTESIAN_POINT('Ctrl Pts',(-40.053516493891,3.22959731636452,2.61892692349575));
#26644=CARTESIAN_POINT('Ctrl Pts',(-40.0404369540956,2.46422838844342,3.35125140856129));
#26645=CARTESIAN_POINT('Ctrl Pts',(-40.0335134405718,2.00806398201211,3.64293615791774));
#26646=CARTESIAN_POINT('Ctrl Pts',(-40.0197190068943,1.00070809848204,4.03885293655703));
#26647=CARTESIAN_POINT('Ctrl Pts',(-40.012987475074,0.457900809079785,4.13570878662521));
#26648=CARTESIAN_POINT('Ctrl Pts',(-40.0010231515811,-0.610513816318687,
4.11291266072887));
#26649=CARTESIAN_POINT('Ctrl Pts',(-39.9947489848203,-1.12619666349221,
4.00255897520987));
#26650=CARTESIAN_POINT('Ctrl Pts',(-39.9813041330625,-2.10360415532423,
3.58895883078212));
#26651=CARTESIAN_POINT('Ctrl Pts',(-39.9743327543442,-2.55378770749458,
3.28389183220121));
#26652=CARTESIAN_POINT('Ctrl Pts',(-39.9610959576698,-3.29947441517994,
2.53006645859444));
#26653=CARTESIAN_POINT('Ctrl Pts',(-39.9553159945307,-3.5926783721241,2.09294620363441));
#26654=CARTESIAN_POINT('Ctrl Pts',(-39.9429023435717,-4.01018999587605,
1.11009823057164));
#26655=CARTESIAN_POINT('Ctrl Pts',(-39.9360273756597,-4.1217821755761,0.569951981661034));
#26656=CARTESIAN_POINT('Ctrl Pts',(-39.9222003792236,-4.12800221666922,
-0.508774703888089));
#26657=CARTESIAN_POINT('Ctrl Pts',(-39.9153844187221,-4.02790805533635,
-1.03692610883357));
#26658=CARTESIAN_POINT('Ctrl Pts',(-39.9025817014483,-3.63412649732825,
-2.02179037792622));
#26659=CARTESIAN_POINT('Ctrl Pts',(-39.8969789036376,-3.34571628854063,
-2.46995843314048));
#26660=CARTESIAN_POINT('Ctrl Pts',(-39.8838786012199,-2.6023047713686,-3.24702630260162));
#26661=CARTESIAN_POINT('Ctrl Pts',(-39.8768396494237,-2.14900926008281,
-3.56327444715444));
#26662=CARTESIAN_POINT('Ctrl Pts',(-39.8631054381929,-1.16447139702274,
-3.99210612797126));
#26663=CARTESIAN_POINT('Ctrl Pts',(-39.8565333777027,-0.645872395426181,
-4.10801194929109));
#26664=CARTESIAN_POINT('Ctrl Pts',(-39.8500212029461,-0.0796584766999726,
-4.12442349205516));
#26665=CARTESIAN_POINT('Ctrl Pts',(-39.8495664599918,-0.0398171398878583,
-4.12499999999999));
#26666=CARTESIAN_POINT('Ctrl Pts',(-39.8491154631359,3.13681525934293E-14,
-4.12499999999999));
#26667=CARTESIAN_POINT('Origin',(-44.,0.,0.));
#26668=CARTESIAN_POINT('',(-39.5316154631359,1.25662602177568E-15,-4.12499999999999));
#26669=CARTESIAN_POINT('',(-39.6109904640031,-5.93380278614818E-15,-4.12499999999999));
#26670=CARTESIAN_POINT('',(-44.,-5.05166804648282E-16,-4.12499999999999));
#26671=CARTESIAN_POINT('Ctrl Pts',(-39.6109904640031,-1.23582119034381E-14,
-4.12499999999999));
#26672=CARTESIAN_POINT('Ctrl Pts',(-39.6120784864535,-0.0960581909754306,
-4.12499999999999));
#26673=CARTESIAN_POINT('Ctrl Pts',(-39.613187837006,-0.19221534304798,-4.12164472355536));
#26674=CARTESIAN_POINT('Ctrl Pts',(-39.620718248277,-0.833175183420811,
-4.07673814098845));
#26675=CARTESIAN_POINT('Ctrl Pts',(-39.6276223981309,-1.36507991359612,
-3.93071543675476));
#26676=CARTESIAN_POINT('Ctrl Pts',(-39.6414459366988,-2.32806042343033,
-3.44650803714958));
#26677=CARTESIAN_POINT('Ctrl Pts',(-39.6482306169486,-2.75243031666917,
-3.1180788842059));
#26678=CARTESIAN_POINT('Ctrl Pts',(-39.6609633880996,-3.45198123824481,
-2.31954745235684));
#26679=CARTESIAN_POINT('Ctrl Pts',(-39.6666039547501,-3.72112298136687,
-1.85734208907042));
#26680=CARTESIAN_POINT('Ctrl Pts',(-39.6797924788468,-4.0751413196876,-0.840996220796809));
#26681=CARTESIAN_POINT('Ctrl Pts',(-39.6868323341888,-4.15057896526983,
-0.294519932982031));
#26682=CARTESIAN_POINT('Ctrl Pts',(-39.7005208192468,-4.08541641084468,
0.77546114537168));
#26683=CARTESIAN_POINT('Ctrl Pts',(-39.7070489185251,-3.95345127565009,
1.28926298594501));
#26684=CARTESIAN_POINT('Ctrl Pts',(-39.7192901280476,-3.4940224803795,2.26012426002136));
#26685=CARTESIAN_POINT('Ctrl Pts',(-39.725639361951,-3.16294286667469,2.70410066801925));
#26686=CARTESIAN_POINT('Ctrl Pts',(-39.7393865290349,-2.35324967764201,
3.43057131862578));
#26687=CARTESIAN_POINT('Ctrl Pts',(-39.746371017253,-1.8849525637005,3.70857900625545));
#26688=CARTESIAN_POINT('Ctrl Pts',(-39.7596585323065,-0.884784462692935,
4.06260984891072));
#26689=CARTESIAN_POINT('Ctrl Pts',(-39.7655098995271,-0.364556442023356,
4.14182727479458));
#26690=CARTESIAN_POINT('Ctrl Pts',(-39.7778388660033,0.702376467574034,
4.10129005906997));
#26691=CARTESIAN_POINT('Ctrl Pts',(-39.784689191451,1.2386225047964,3.97236936493211));
#26692=CARTESIAN_POINT('Ctrl Pts',(-39.7985157764843,2.21803952075457,3.51856869125415));
#26693=CARTESIAN_POINT('Ctrl Pts',(-39.8053550443527,2.65387954852039,3.20264779831331));
#26694=CARTESIAN_POINT('Ctrl Pts',(-39.818212292288,3.37668007672995,2.42717394157867));
#26695=CARTESIAN_POINT('Ctrl Pts',(-39.8237976592278,3.65873908869338,1.97655506891192));
#26696=CARTESIAN_POINT('Ctrl Pts',(-39.8368277047136,4.0457284357555,0.973721948313611));
#26697=CARTESIAN_POINT('Ctrl Pts',(-39.8438643444358,4.13917345088107,0.428125310920622));
#26698=CARTESIAN_POINT('Ctrl Pts',(-39.857631459975,4.10795416376912,-0.646803641311481));
#26699=CARTESIAN_POINT('Ctrl Pts',(-39.864236648442,3.99173323773183,-1.16606865962808));
#26700=CARTESIAN_POINT('Ctrl Pts',(-39.8766147511517,3.56403405226136,-2.14649961709799));
#26701=CARTESIAN_POINT('Ctrl Pts',(-39.8826941077983,3.25123200088449,-2.59601571084602));
#26702=CARTESIAN_POINT('Ctrl Pts',(-39.8962967627661,2.47043449902232,-3.34747094998367));
#26703=CARTESIAN_POINT('Ctrl Pts',(-39.9033070700102,2.01034235308391,-3.64240738946468));
#26704=CARTESIAN_POINT('Ctrl Pts',(-39.9166344383974,1.02646869575269,-4.02837734110635));
#26705=CARTESIAN_POINT('Ctrl Pts',(-39.9226518744084,0.51547130702924,-4.12499999951931));
#26706=CARTESIAN_POINT('Ctrl Pts',(-39.9284904639595,3.84657155935038E-9,
-4.12499999999999));
#26707=CARTESIAN_POINT('Ctrl Pts',(-39.8491154631359,3.13681525934293E-14,
-4.12499999999999));
#26708=CARTESIAN_POINT('Ctrl Pts',(-39.843402485096,0.504381444880162,-4.12499999999999));
#26709=CARTESIAN_POINT('Ctrl Pts',(-39.8375223233553,1.00487152049101,-4.03248595035866));
#26710=CARTESIAN_POINT('Ctrl Pts',(-39.8243576494017,1.98112817703027,-3.65825910161386));
#26711=CARTESIAN_POINT('Ctrl Pts',(-39.8173576492924,2.44288280604376,-3.36749940249));
#26712=CARTESIAN_POINT('Ctrl Pts',(-39.8040027808205,3.21427799065912,-2.63744746711315));
#26713=CARTESIAN_POINT('Ctrl Pts',(-39.7980384429505,3.52170140820749,-2.21027615043971));
#26714=CARTESIAN_POINT('Ctrl Pts',(-39.7858240655497,3.97135752656289,-1.24184905854371));
#26715=CARTESIAN_POINT('Ctrl Pts',(-39.7790089067465,4.10070484310535,-0.705747913315952));
#26716=CARTESIAN_POINT('Ctrl Pts',(-39.7651872213033,4.1426232649795,0.373811128262174));
#26717=CARTESIAN_POINT('Ctrl Pts',(-39.7583187121852,4.05943945848419,0.906651862177761));
#26718=CARTESIAN_POINT('Ctrl Pts',(-39.7453894698742,3.69757339961626,1.90249963232007));
#26719=CARTESIAN_POINT('Ctrl Pts',(-39.7398105076248,3.42551234676977,2.35741774652478));
#26720=CARTESIAN_POINT('Ctrl Pts',(-39.7268751988628,2.70944016452086,3.15850728351391));
#26721=CARTESIAN_POINT('Ctrl Pts',(-39.7198438075971,2.26532985103266,3.49077489483737));
#26722=CARTESIAN_POINT('Ctrl Pts',(-39.7060370101051,1.29206995435841,3.95286983078476));
#26723=CARTESIAN_POINT('Ctrl Pts',(-39.6993896596857,0.775810073068537,
4.08567630966704));
#26724=CARTESIAN_POINT('Ctrl Pts',(-39.6869335551,-0.28970140984737,4.14999731159824));
#26725=CARTESIAN_POINT('Ctrl Pts',(-39.68098416215,-0.829144441797188,4.07663213774457));
#26726=CARTESIAN_POINT('Ctrl Pts',(-39.6674677452171,-1.85215882006829,
3.72549080996463));
#26727=CARTESIAN_POINT('Ctrl Pts',(-39.66044621068,-2.3254103729873,3.44996225448759));
#26728=CARTESIAN_POINT('Ctrl Pts',(-39.6469735531507,-3.12320577978043,
2.74483237311875));
#26729=CARTESIAN_POINT('Ctrl Pts',(-39.6407591472535,-3.44536102340515,
2.32765735044714));
#26730=CARTESIAN_POINT('Ctrl Pts',(-39.6287515009935,-3.9275052950731,1.37422083235662));
#26731=CARTESIAN_POINT('Ctrl Pts',(-39.6220048306236,-4.07472638121562,
0.8428376377412));
#26732=CARTESIAN_POINT('Ctrl Pts',(-39.6082041013904,-4.15295732985394,
-0.236354875145553));
#26733=CARTESIAN_POINT('Ctrl Pts',(-39.6012892767861,-4.08714456180461,
-0.773414839596819));
#26734=CARTESIAN_POINT('Ctrl Pts',(-39.5882351301151,-3.7577282036435,-1.78013835225203));
#26735=CARTESIAN_POINT('Ctrl Pts',(-39.5826206126713,-3.50185985590037,
-2.24196104421186));
#26736=CARTESIAN_POINT('Ctrl Pts',(-39.5698551236704,-2.81333837034102,
-3.06666841839316));
#26737=CARTESIAN_POINT('Ctrl Pts',(-39.5628389099864,-2.37893526329097,
-3.41467248922035));
#26738=CARTESIAN_POINT('Ctrl Pts',(-39.548973667415,-1.41801473088533,-3.90967882644601));
#26739=CARTESIAN_POINT('Ctrl Pts',(-39.5422575317382,-0.904628541834916,
-4.05931128723266));
#26740=CARTESIAN_POINT('Ctrl Pts',(-39.5344981490777,-0.2514509148248,-4.11925879260599));
#26741=CARTESIAN_POINT('Ctrl Pts',(-39.5330386994699,-0.125653204598835,
-4.12499999999999));
#26742=CARTESIAN_POINT('Ctrl Pts',(-39.5316154631359,-1.16920362280837E-14,
-4.12499999999999));
#26743=CARTESIAN_POINT('Origin',(-44.,0.,0.));
#26744=CARTESIAN_POINT('',(-39.2141154631359,7.39754712673358E-15,-4.12499999999999));
#26745=CARTESIAN_POINT('',(-39.2934904648176,-3.59547304179607E-8,-4.12499999999999));
#26746=CARTESIAN_POINT('',(-44.,-5.05166804648282E-16,-4.12499999999999));
#26747=CARTESIAN_POINT('Ctrl Pts',(-39.2934904644104,-3.5959404204311E-8,
-4.12499999999999));
#26748=CARTESIAN_POINT('Ctrl Pts',(-39.295599384249,-0.186190149588254,
-4.12499999837689));
#26749=CARTESIAN_POINT('Ctrl Pts',(-39.2977861373005,-0.372549332322611,
-4.11239426138431));
#26750=CARTESIAN_POINT('Ctrl Pts',(-39.3066474723105,-1.10195949492571,
-4.01284715042124));
#26751=CARTESIAN_POINT('Ctrl Pts',(-39.3136787388404,-1.62585126307851,
-3.83064734391326));
#26752=CARTESIAN_POINT('Ctrl Pts',(-39.3274862514165,-2.55341291536397,
-3.28248777516562));
#26753=CARTESIAN_POINT('Ctrl Pts',(-39.3341343886972,-2.95234017512007,
-2.92888007643203));
#26754=CARTESIAN_POINT('Ctrl Pts',(-39.3465919737327,-3.60175656712804,
-2.0817522056745));
#26755=CARTESIAN_POINT('Ctrl Pts',(-39.3525390739346,-3.84273753841753,
-1.59364873374324));
#26756=CARTESIAN_POINT('Ctrl Pts',(-39.3660538272193,-4.12408110394775,
-0.549319041224531));
#26757=CARTESIAN_POINT('Ctrl Pts',(-39.3730755497843,-4.16050319778585,
-0.00289466185195243));
#26758=CARTESIAN_POINT('Ctrl Pts',(-39.3865494573202,-4.02243009077466,
1.05289540411226));
#26759=CARTESIAN_POINT('Ctrl Pts',(-39.3927668921141,-3.85690107642523,
1.55332829300766));
#26760=CARTESIAN_POINT('Ctrl Pts',(-39.4047722979627,-3.33640726107213,
2.48639624480013));
#26761=CARTESIAN_POINT('Ctrl Pts',(-39.4115181919553,-2.97834694191541,
2.90572173604516));
#26762=CARTESIAN_POINT('Ctrl Pts',(-39.4253186114539,-2.12762856695797,
3.5743719592753));
#26763=CARTESIAN_POINT('Ctrl Pts',(-39.4322338938875,-1.6456533410096,3.82030970791316));
#26764=CARTESIAN_POINT('Ctrl Pts',(-39.4452893602645,-0.626933783143563,
4.11051693858186));
#26765=CARTESIAN_POINT('Ctrl Pts',(-39.4509045795661,-0.10101988185248,
4.15682431718069));
#26766=CARTESIAN_POINT('Ctrl Pts',(-39.4636682366469,0.967751936535434,
4.04756798604883));
#26767=CARTESIAN_POINT('Ctrl Pts',(-39.4706842480285,1.49925370884556,3.88221353574909));
#26768=CARTESIAN_POINT('Ctrl Pts',(-39.4845500362765,2.44718453842596,3.362686514528));
#26769=CARTESIAN_POINT('Ctrl Pts',(-39.4912668685653,2.85844670521885,3.02087103436019));
#26770=CARTESIAN_POINT('Ctrl Pts',(-39.5038578262864,3.53195717667501,2.19691185348038));
#26771=CARTESIAN_POINT('Ctrl Pts',(-39.5096259671741,3.78654151503228,1.72140910431719));
#26772=CARTESIAN_POINT('Ctrl Pts',(-39.5229867970177,4.10308374097648,0.690314646312808));
#26773=CARTESIAN_POINT('Ctrl Pts',(-39.5300215415094,4.15827215547997,0.143529887484189));
#26774=CARTESIAN_POINT('Ctrl Pts',(-39.5436055190979,4.05516751064371,-0.919624546867021));
#26775=CARTESIAN_POINT('Ctrl Pts',(-39.5500395984354,3.90571629799609,-1.42670343379841));
#26776=CARTESIAN_POINT('Ctrl Pts',(-39.5620085730998,3.41491132232603,-2.37742599538191));
#26777=CARTESIAN_POINT('Ctrl Pts',(-39.568601290936,3.07056680412132,-2.80809809184484));
#26778=CARTESIAN_POINT('Ctrl Pts',(-39.5823680755418,2.24055924177556,-3.50494474729392));
#26779=CARTESIAN_POINT('Ctrl Pts',(-39.5893210568637,1.76509769813185,-3.76685218921186));
#26780=CARTESIAN_POINT('Ctrl Pts',(-39.6012960044861,0.847192453867817,
-4.05944841020172));
#26781=CARTESIAN_POINT('Ctrl Pts',(-39.60618153575,0.424565640489271,-4.12499999999999));
#26782=CARTESIAN_POINT('Ctrl Pts',(-39.6109904640031,-1.23582119034381E-14,
-4.12499999999999));
#26783=CARTESIAN_POINT('Ctrl Pts',(-39.5316154631359,-1.28833483865871E-14,
-4.12499999999999));
#26784=CARTESIAN_POINT('Ctrl Pts',(-39.5270062407276,0.406934219222845,
-4.12499999999999));
#26785=CARTESIAN_POINT('Ctrl Pts',(-39.5223363198912,0.812347824891932,
-4.06477965010671));
#26786=CARTESIAN_POINT('Ctrl Pts',(-39.5105357603151,1.72348496276242,-3.78700521349252));
#26787=CARTESIAN_POINT('Ctrl Pts',(-39.5035011115944,2.20753977941869,-3.52683635719434));
#26788=CARTESIAN_POINT('Ctrl Pts',(-39.4899182410904,3.03101153407769,-2.84658455385363));
#26789=CARTESIAN_POINT('Ctrl Pts',(-39.4834851202791,3.3676748191655,-2.43902654846832));
#26790=CARTESIAN_POINT('Ctrl Pts',(-39.4715186405353,3.88107743642454,-1.50033645743129));
#26791=CARTESIAN_POINT('Ctrl Pts',(-39.4649229943107,4.04538718282125,-0.97397940572874));
#26792=CARTESIAN_POINT('Ctrl Pts',(-39.4511558042648,4.15859905583844,0.103818602234392));
#26793=CARTESIAN_POINT('Ctrl Pts',(-39.4442031826834,4.10967803484536,0.644416613965508));
#26794=CARTESIAN_POINT('Ctrl Pts',(-39.4310322347819,3.8115726491491,1.66134405757424));
#26795=CARTESIAN_POINT('Ctrl Pts',(-39.4253281053926,3.57095108017744,2.12989537645652));
#26796=CARTESIAN_POINT('Ctrl Pts',(-39.4128064587927,2.91287926763723,2.97138178254049));
#26797=CARTESIAN_POINT('Ctrl Pts',(-39.4059017891302,2.49426416236043,3.33055759347151));
#26798=CARTESIAN_POINT('Ctrl Pts',(-39.3920783566002,1.5541855677181,3.85781962416697));
#26799=CARTESIAN_POINT('Ctrl Pts',(-39.3852942749978,1.04456260395922,4.02581166954861));
#26800=CARTESIAN_POINT('Ctrl Pts',(-39.3725628105428,-0.00869603853111918,
4.15889866115016));
#26801=CARTESIAN_POINT('Ctrl Pts',(-39.3669213767033,-0.542409605992354,
4.12338532663788));
#26802=CARTESIAN_POINT('Ctrl Pts',(-39.3537312247787,-1.58288504110619,
3.84818211866607));
#26803=CARTESIAN_POINT('Ctrl Pts',(-39.346691374359,-2.07801866231148,3.60497786987691));
#26804=CARTESIAN_POINT('Ctrl Pts',(-39.3330037806798,-2.92838982685494,
2.95236901937931));
#26805=CARTESIAN_POINT('Ctrl Pts',(-39.3264765181129,-3.2804161839462,2.55554852638602));
#26806=CARTESIAN_POINT('Ctrl Pts',(-39.3142367598118,-3.82811724441854,
1.63154730083484));
#26807=CARTESIAN_POINT('Ctrl Pts',(-39.3078843912774,-4.01089579172321,
1.10867329980487));
#26808=CARTESIAN_POINT('Ctrl Pts',(-39.2941357396797,-4.16000209505153,
0.0310678347067559));
#26809=CARTESIAN_POINT('Ctrl Pts',(-39.2871515658459,-4.12841714503876,
-0.512596650218839));
#26810=CARTESIAN_POINT('Ctrl Pts',(-39.2738653240342,-3.86227563484386,
-1.5396332532564));
#26811=CARTESIAN_POINT('Ctrl Pts',(-39.2680158909314,-3.636872729621,-2.01514085728428));
#26812=CARTESIAN_POINT('Ctrl Pts',(-39.2556847820188,-3.00633714628252,
-2.87677781179184));
#26813=CARTESIAN_POINT('Ctrl Pts',(-39.2488338188269,-2.59945910740675,
-3.24911021753748));
#26814=CARTESIAN_POINT('Ctrl Pts',(-39.2350071893406,-1.67537468047583,
-3.80698373692771));
#26815=CARTESIAN_POINT('Ctrl Pts',(-39.2281684931446,-1.16969888523996,
-3.99146773122192));
#26816=CARTESIAN_POINT('Ctrl Pts',(-39.2190847694358,-0.429801702513547,
-4.1082178495998));
#26817=CARTESIAN_POINT('Ctrl Pts',(-39.21654878163,-0.214830284541508,-4.12499999999999));
#26818=CARTESIAN_POINT('Ctrl Pts',(-39.2141154631359,3.40005801291454E-14,
-4.12499999999999));
#26819=CARTESIAN_POINT('Origin',(-44.,0.,0.));
#26820=CARTESIAN_POINT('',(-38.8966154631359,-7.81597775758302E-15,-4.12499999999999));
#26821=CARTESIAN_POINT('',(-38.9759904640031,-5.04042019602013E-15,-4.12499999999999));
#26822=CARTESIAN_POINT('',(-44.,-5.05166804648282E-16,-4.12499999999999));
#26823=CARTESIAN_POINT('Ctrl Pts',(-38.9759904640031,-2.15105711021124E-14,
-4.12499999999999));
#26824=CARTESIAN_POINT('Ctrl Pts',(-38.9790474996013,-0.269896369513169,
-4.12499999999999));
#26825=CARTESIAN_POINT('Ctrl Pts',(-38.9822635574637,-0.539748106423213,
-4.09851142651325));
#26826=CARTESIAN_POINT('Ctrl Pts',(-38.992171577137,-1.33074276654309,-3.94099260355166));
#26827=CARTESIAN_POINT('Ctrl Pts',(-38.9990717182805,-1.83050192552105,
-3.73517849360003));
#26828=CARTESIAN_POINT('Ctrl Pts',(-39.0128811969529,-2.73228840497834,
-3.1382164174264));
#26829=CARTESIAN_POINT('Ctrl Pts',(-39.019651620186,-3.12327088774582,-2.74936196462474));
#26830=CARTESIAN_POINT('Ctrl Pts',(-39.0317288442979,-3.71769260733261,
-1.86196066114348));
#26831=CARTESIAN_POINT('Ctrl Pts',(-39.0378525559747,-3.92326379015565,
-1.37700840925209));
#26832=CARTESIAN_POINT('Ctrl Pts',(-39.0512861088709,-4.14674799464015,
-0.336991875673695));
#26833=CARTESIAN_POINT('Ctrl Pts',(-39.0583013204775,-4.15512014108993,
0.209904172918947));
#26834=CARTESIAN_POINT('Ctrl Pts',(-39.0718690354137,-3.96014727794907,
1.27499822485171));
#26835=CARTESIAN_POINT('Ctrl Pts',(-39.077893072742,-3.75894753442914,1.78288911644535));
#26836=CARTESIAN_POINT('Ctrl Pts',(-39.0903030835144,-3.17925708982892,
2.68074128890209));
#26837=CARTESIAN_POINT('Ctrl Pts',(-39.0969256833317,-2.81063365599906,
3.06502531008103));
#26838=CARTESIAN_POINT('Ctrl Pts',(-39.1107095013912,-1.93156464744709,
3.68586291261577));
#26839=CARTESIAN_POINT('Ctrl Pts',(-39.117744304952,-1.42484137660058,3.90977743641053));
#26840=CARTESIAN_POINT('Ctrl Pts',(-39.1307359923122,-0.375402464839822,
4.14144133452341));
#26841=CARTESIAN_POINT('Ctrl Pts',(-39.1363164342365,0.155364053080466,
4.15551749008611));
#26842=CARTESIAN_POINT('Ctrl Pts',(-39.1492030408596,1.20094621231838,3.98223276667685));
#26843=CARTESIAN_POINT('Ctrl Pts',(-39.1560544478221,1.70554863977671,3.79361951957827));
#26844=CARTESIAN_POINT('Ctrl Pts',(-39.1698796448005,2.62545931848446,3.22813418022329));
#26845=CARTESIAN_POINT('Ctrl Pts',(-39.1767159975248,3.02932345921329,2.85255943133749));
#26846=CARTESIAN_POINT('Ctrl Pts',(-39.1889986252139,3.65291444704421,1.98591158993573));
#26847=CARTESIAN_POINT('Ctrl Pts',(-39.1948934325522,3.87449493902384,1.50861745452681));
#26848=CARTESIAN_POINT('Ctrl Pts',(-39.2082083611995,4.13250053218192,0.479059158036542));
#26849=CARTESIAN_POINT('Ctrl Pts',(-39.215199430204,4.15966272975775,-0.065297597988825));
#26850=CARTESIAN_POINT('Ctrl Pts',(-39.2289143087603,4.00173529390893,-1.14057679742806));
#26851=CARTESIAN_POINT('Ctrl Pts',(-39.2351972511196,3.81540734251379,-1.66055888320928));
#26852=CARTESIAN_POINT('Ctrl Pts',(-39.2476992999592,3.25123845070424,-2.59678981543789));
#26853=CARTESIAN_POINT('Ctrl Pts',(-39.2545137578529,2.87926912340319,-3.0039422018544));
#26854=CARTESIAN_POINT('Ctrl Pts',(-39.2683353001993,2.00793250615844,-3.64270357598583));
#26855=CARTESIAN_POINT('Ctrl Pts',(-39.2752043497793,1.51973610071058,-3.87188436109807));
#26856=CARTESIAN_POINT('Ctrl Pts',(-39.2858533066883,0.673253899371989,
-4.08372402589253));
#26857=CARTESIAN_POINT('Ctrl Pts',(-39.2896744394388,0.336905193941784,
-4.12500000293694));
#26858=CARTESIAN_POINT('Ctrl Pts',(-39.2934904644104,-3.59594048395727E-8,
-4.12499999999999));
#26859=CARTESIAN_POINT('Ctrl Pts',(-39.2141154631359,3.13681525934293E-14,
-4.12499999999999));
#26860=CARTESIAN_POINT('Ctrl Pts',(-39.2106076395524,0.309695068855631,
-4.12499999999999));
#26861=CARTESIAN_POINT('Ctrl Pts',(-39.2071110024133,0.619094537650788,
-4.09012254664969));
#26862=CARTESIAN_POINT('Ctrl Pts',(-39.196695117648,1.45649361160747,-3.89803246967592));
#26863=CARTESIAN_POINT('Ctrl Pts',(-39.189658402646,1.96096703584027,-3.67023625977947));
#26864=CARTESIAN_POINT('Ctrl Pts',(-39.175892081298,2.83441544551272,-3.04297763892349));
#26865=CARTESIAN_POINT('Ctrl Pts',(-39.1692877099202,3.19977026976349,-2.65614420856511));
#26866=CARTESIAN_POINT('Ctrl Pts',(-39.1569110947223,3.77313686189122,-1.75308434849624));
#26867=CARTESIAN_POINT('Ctrl Pts',(-39.1508290874092,3.970725038286,-1.24226285192036));
#26868=CARTESIAN_POINT('Ctrl Pts',(-39.1372248150422,4.15669220016776,-0.174631796483549));
#26869=CARTESIAN_POINT('Ctrl Pts',(-39.1302147468664,4.14372093648504,0.371702458396875));
#26870=CARTESIAN_POINT('Ctrl Pts',(-39.1168097438426,3.91179105654006,1.40919716469096));
#26871=CARTESIAN_POINT('Ctrl Pts',(-39.1107473679707,3.70233301351323,1.89226394095644));
#26872=CARTESIAN_POINT('Ctrl Pts',(-39.0986199515878,3.10081981753944,2.77466222329187));
#26873=CARTESIAN_POINT('Ctrl Pts',(-39.0918328310287,2.70667356357166,3.16033897225272));
#26874=CARTESIAN_POINT('Ctrl Pts',(-39.0780180998527,1.80039426427184,3.74972342793978));
#26875=CARTESIAN_POINT('Ctrl Pts',(-39.0711291166307,1.29940843771414,3.95137781008399));
#26876=CARTESIAN_POINT('Ctrl Pts',(-39.0581465698181,0.258893382924898,
4.15012262690843));
#26877=CARTESIAN_POINT('Ctrl Pts',(-39.052559819976,-0.270180862102667,
4.14940293972721));
#26878=CARTESIAN_POINT('Ctrl Pts',(-39.039696128115,-1.32487355405879,3.94497537962508));
#26879=CARTESIAN_POINT('Ctrl Pts',(-39.0326702602678,-1.83847358117235,
3.73338043732847));
#26880=CARTESIAN_POINT('Ctrl Pts',(-39.018836886592,-2.73488704715773,3.13300998511365));
#26881=CARTESIAN_POINT('Ctrl Pts',(-39.0121594953428,-3.11365616207528,
2.75690245931389));
#26882=CARTESIAN_POINT('Ctrl Pts',(-38.9996461566451,-3.71307058463043,
1.87541539377217));
#26883=CARTESIAN_POINT('Ctrl Pts',(-38.9937805709011,-3.92545063473447,
1.3765600433662));
#26884=CARTESIAN_POINT('Ctrl Pts',(-38.9803291922002,-4.14831505802596,
0.319566254637141));
#26885=CARTESIAN_POINT('Ctrl Pts',(-38.9733010780177,-4.15430764739794,
-0.228837826006839));
#26886=CARTESIAN_POINT('Ctrl Pts',(-38.9597803760164,-3.95720546520464,
-1.27657329396925));
#26887=CARTESIAN_POINT('Ctrl Pts',(-38.9534436245317,-3.76366253628105,
-1.76746632844331));
#26888=CARTESIAN_POINT('Ctrl Pts',(-38.9415228464317,-3.19120408915522,
-2.67019767817732));
#26889=CARTESIAN_POINT('Ctrl Pts',(-38.9348067953756,-2.81014340061275,
-3.06868415908844));
#26890=CARTESIAN_POINT('Ctrl Pts',(-38.9210193349198,-1.92261251543051,
-3.6888011243803));
#26891=CARTESIAN_POINT('Ctrl Pts',(-38.9140874341518,-1.426848744064,-3.90740294846574));
#26892=CARTESIAN_POINT('Ctrl Pts',(-38.9036813911272,-0.606059342712801,
-4.09157961116413));
#26893=CARTESIAN_POINT('Ctrl Pts',(-38.9000492507543,-0.303158658804201,
-4.12499999999999));
#26894=CARTESIAN_POINT('Ctrl Pts',(-38.8966154631359,-1.16573417585641E-14,
-4.12499999999999));
#26895=CARTESIAN_POINT('Origin',(-44.,0.,0.));
#26896=CARTESIAN_POINT('',(-38.5791154631359,-1.5969178094674E-14,-4.12499999999999));
#26897=CARTESIAN_POINT('',(-38.6584904640031,5.29853172080164E-15,-4.12499999999999));
#26898=CARTESIAN_POINT('',(-44.,-5.05166804648282E-16,-4.12499999999999));
#26899=CARTESIAN_POINT('Ctrl Pts',(-38.6584904640031,-1.74860126378462E-14,
-4.12499999999999));
#26900=CARTESIAN_POINT('Ctrl Pts',(-38.6625193640772,-0.35569932642004,
-4.12499999999999));
#26901=CARTESIAN_POINT('Ctrl Pts',(-38.666816404744,-0.710608137653691,
-4.07899022355685));
#26902=CARTESIAN_POINT('Ctrl Pts',(-38.6780065172728,-1.57663101836591,
-3.8496956268941));
#26903=CARTESIAN_POINT('Ctrl Pts',(-38.6849802916811,-2.06544662779795,
-3.61107336014592));
#26904=CARTESIAN_POINT('Ctrl Pts',(-38.6987754840373,-2.93308426250075,
-2.95225879949218));
#26905=CARTESIAN_POINT('Ctrl Pts',(-38.7052301010454,-3.30053012312115,
-2.53481766159836));
#26906=CARTESIAN_POINT('Ctrl Pts',(-38.717423849814,-3.83713355243541,-1.60244055093468));
#26907=CARTESIAN_POINT('Ctrl Pts',(-38.7239243883266,-4.00977089429739,
-1.10142541046586));
#26908=CARTESIAN_POINT('Ctrl Pts',(-38.7375831250835,-4.16072925823174,
-0.0413118164422865));
#26909=CARTESIAN_POINT('Ctrl Pts',(-38.7446224123957,-4.12970481913612,
0.50883790280608));
#26910=CARTESIAN_POINT('Ctrl Pts',(-38.7578636131338,-3.85899534969774,
1.55110853918749));
#26911=CARTESIAN_POINT('Ctrl Pts',(-38.7635354456736,-3.62740470376424,
2.0346293191332));
#26912=CARTESIAN_POINT('Ctrl Pts',(-38.7762256240908,-2.99364950257224,
2.88717331827899));
#26913=CARTESIAN_POINT('Ctrl Pts',(-38.782990529657,-2.59743470686741,3.24823554430925));
#26914=CARTESIAN_POINT('Ctrl Pts',(-38.7968098485576,-1.67700368856532,
3.80810237752584));
#26915=CARTESIAN_POINT('Ctrl Pts',(-38.8037304728962,-1.15856033930691,
3.99646473989038));
#26916=CARTESIAN_POINT('Ctrl Pts',(-38.816313351069,-0.102058589372211,
4.15668864362566));
#26917=CARTESIAN_POINT('Ctrl Pts',(-38.8219822057465,0.424592352730211,
4.13620612943619));
#26918=CARTESIAN_POINT('Ctrl Pts',(-38.8351152300092,1.45659591667997,3.89646770657547));
#26919=CARTESIAN_POINT('Ctrl Pts',(-38.8420561961729,1.95105063724238,3.67389866493515));
#26920=CARTESIAN_POINT('Ctrl Pts',(-38.8558353355033,2.8340425270065,3.04662676057572));
#26921=CARTESIAN_POINT('Ctrl Pts',(-38.8625255368819,3.21196550207653,2.64518131664316));
#26922=CARTESIAN_POINT('Ctrl Pts',(-38.8744131495901,3.77755565123565,1.73769514038321));
#26923=CARTESIAN_POINT('Ctrl Pts',(-38.8808158529087,3.96732924442539,1.2449095827013));
#26924=CARTESIAN_POINT('Ctrl Pts',(-38.8943631979186,4.15610184752558,0.194805077521741));
#26925=CARTESIAN_POINT('Ctrl Pts',(-38.9013943947845,4.14557826576012,-0.353997679006895));
#26926=CARTESIAN_POINT('Ctrl Pts',(-38.9148084184843,3.91398593596523,-1.4083825527151));
#26927=CARTESIAN_POINT('Ctrl Pts',(-38.9206311516536,3.69810657045983,-1.90442421215133));
#26928=CARTESIAN_POINT('Ctrl Pts',(-38.9331767909217,3.09247613130066,-2.78071508509055));
#26929=CARTESIAN_POINT('Ctrl Pts',(-38.939870782221,2.71052692038369,-3.15417531195753));
#26930=CARTESIAN_POINT('Ctrl Pts',(-38.9537181636733,1.80870958177029,-3.74795834727925));
#26931=CARTESIAN_POINT('Ctrl Pts',(-38.9607402669324,1.29298833288854,-3.95560484262641));
#26932=CARTESIAN_POINT('Ctrl Pts',(-38.9703269021749,0.50324821785069,-4.10198003830776));
#26933=CARTESIAN_POINT('Ctrl Pts',(-38.9731406059396,0.251605295474299,
-4.12499999999999));
#26934=CARTESIAN_POINT('Ctrl Pts',(-38.9759904640031,-1.23582119034381E-14,
-4.12499999999999));
#26935=CARTESIAN_POINT('Ctrl Pts',(-38.8966154631359,-1.28833483865871E-14,
-4.12499999999999));
#26936=CARTESIAN_POINT('Ctrl Pts',(-38.8941551257047,0.217215704275863,
-4.12499999999999));
#26937=CARTESIAN_POINT('Ctrl Pts',(-38.8917389813284,0.434563195301831,
-4.10784292032265));
#26938=CARTESIAN_POINT('Ctrl Pts',(-38.8827081392599,1.18941421738817,-3.98739239222705));
#26939=CARTESIAN_POINT('Ctrl Pts',(-38.8757761772874,1.7063965454856,-3.79502410638837));
#26940=CARTESIAN_POINT('Ctrl Pts',(-38.8619608831417,2.62214532974901,-3.22825618620668));
#26941=CARTESIAN_POINT('Ctrl Pts',(-38.8552106323992,3.01531105470513,-2.8644701966738));
#26942=CARTESIAN_POINT('Ctrl Pts',(-38.8425513085925,3.64301874167191,-2.00678695994037));
#26943=CARTESIAN_POINT('Ctrl Pts',(-38.8368530051158,3.87124617766612,-1.52060326836833));
#26944=CARTESIAN_POINT('Ctrl Pts',(-38.8235741401363,4.13359596934735,-0.475686737312476));
#26945=CARTESIAN_POINT('Ctrl Pts',(-38.8165357861214,4.16021387590477,0.0742363049878281));
#26946=CARTESIAN_POINT('Ctrl Pts',(-38.8028994855135,4.00110661022955,1.13231530738008));
#26947=CARTESIAN_POINT('Ctrl Pts',(-38.7964192791794,3.82476576207119,1.63161520311227));
#26948=CARTESIAN_POINT('Ctrl Pts',(-38.7843295174402,3.28362068269884,2.55572269933035));
#26949=CARTESIAN_POINT('Ctrl Pts',(-38.777873816786,2.9167823001544,2.96753795432328));
#26950=CARTESIAN_POINT('Ctrl Pts',(-38.7641287818026,2.05008100550226,3.61978520293195));
#26951=CARTESIAN_POINT('Ctrl Pts',(-38.7571590663949,1.56047246954954,3.85624222065994));
#26952=CARTESIAN_POINT('Ctrl Pts',(-38.7439283948578,0.534412161839448,
4.12337198936735));
#26953=CARTESIAN_POINT('Ctrl Pts',(-38.7381562807806,0.00916916585072175,
4.15784836567742));
#26954=CARTESIAN_POINT('Ctrl Pts',(-38.7257324925636,-1.05056311073634,
4.02619700780108));
#26955=CARTESIAN_POINT('Ctrl Pts',(-38.7188546534834,-1.57384711308623,
3.85187515299262));
#26956=CARTESIAN_POINT('Ctrl Pts',(-38.7050277946806,-2.51017981893487,
3.31634719660548));
#26957=CARTESIAN_POINT('Ctrl Pts',(-38.698214722834,-2.91687171763236,2.96496643205763));
#26958=CARTESIAN_POINT('Ctrl Pts',(-38.6854186111024,-3.57158157041546,
2.13037376857811));
#26959=CARTESIAN_POINT('Ctrl Pts',(-38.6798129800651,-3.8147745344501,1.65595381201699));
#26960=CARTESIAN_POINT('Ctrl Pts',(-38.6667042550831,-4.11423373550093,
0.62301235783989));
#26961=CARTESIAN_POINT('Ctrl Pts',(-38.6596651194103,-4.16050790034444,
0.0723419343465299));
#26962=CARTESIAN_POINT('Ctrl Pts',(-38.6459350583739,-4.03783829815713,
-0.994322838177824));
#26963=CARTESIAN_POINT('Ctrl Pts',(-38.6393670794612,-3.87810220559565,
-1.50104886972644));
#26964=CARTESIAN_POINT('Ctrl Pts',(-38.6270558816207,-3.36781647438429,
-2.44350607415521));
#26965=CARTESIAN_POINT('Ctrl Pts',(-38.6208510972024,-3.01570572680273,
-2.86678197462549));
#26966=CARTESIAN_POINT('Ctrl Pts',(-38.6071767129135,-2.1710764440728,-3.5488095434222));
#26967=CARTESIAN_POINT('Ctrl Pts',(-38.6001780673964,-1.68802106886808,
-3.80239492397942));
#26968=CARTESIAN_POINT('Ctrl Pts',(-38.5883995110342,-0.789429385568951,
-4.06814385357856));
#26969=CARTESIAN_POINT('Ctrl Pts',(-38.5835941021609,-0.39540540970529,
-4.12499999999999));
#26970=CARTESIAN_POINT('Ctrl Pts',(-38.5791154631359,-6.57113252700015E-14,
-4.12499999999999));
#26971=CARTESIAN_POINT('Origin',(-44.,0.,0.));
#26972=CARTESIAN_POINT('',(-38.261615463136,-6.99207366342899E-13,-4.12499999999999));
#26973=CARTESIAN_POINT('',(-38.3409904640031,-2.68119626869167E-15,-4.12499999999999));
#26974=CARTESIAN_POINT('',(-44.,-5.05166804648282E-16,-4.12499999999999));
#26975=CARTESIAN_POINT('Ctrl Pts',(-38.3409904640031,2.84494650060196E-14,
-4.12499999999999));
#26976=CARTESIAN_POINT('Ctrl Pts',(-38.3460731333721,-0.448733410539718,
-4.12499999999999));
#26977=CARTESIAN_POINT('Ctrl Pts',(-38.3515687489139,-0.894988901034538,
-4.05177263444848));
#26978=CARTESIAN_POINT('Ctrl Pts',(-38.3641290304286,-1.83494582066274,
-3.7340199284862));
#26979=CARTESIAN_POINT('Ctrl Pts',(-38.3711518773069,-2.30958973180772,
-3.46059640334447));
#26980=CARTESIAN_POINT('Ctrl Pts',(-38.3846564814364,-3.12306575806814,
-2.74816899221892));
#26981=CARTESIAN_POINT('Ctrl Pts',(-38.3905897661896,-3.45496107975674,
-2.31715585160993));
#26982=CARTESIAN_POINT('Ctrl Pts',(-38.4030563636754,-3.92957274116637,
-1.36133166666959));
#26983=CARTESIAN_POINT('Ctrl Pts',(-38.4097092800234,-4.071454835502,-0.847357016752972));
#26984=CARTESIAN_POINT('Ctrl Pts',(-38.4235211144765,-4.15521847085631,
0.22704473077945));
#26985=CARTESIAN_POINT('Ctrl Pts',(-38.4305516010864,-4.0880889406769,0.777768810425782));
#26986=CARTESIAN_POINT('Ctrl Pts',(-38.4434739145985,-3.749699355543,1.79752959830024));
#26987=CARTESIAN_POINT('Ctrl Pts',(-38.4490534938235,-3.49067077741897,
2.25977347387685));
#26988=CARTESIAN_POINT('Ctrl Pts',(-38.4619924785919,-2.80719285316213,
3.06934466299846));
#26989=CARTESIAN_POINT('Ctrl Pts',(-38.4688648061341,-2.38636786388807,
3.40682445000972));
#26990=CARTESIAN_POINT('Ctrl Pts',(-38.4826854358763,-1.42907319461139,
3.9078899385387));
#26991=CARTESIAN_POINT('Ctrl Pts',(-38.4894955993512,-0.899727126113582,
4.06255516959346));
#26992=CARTESIAN_POINT('Ctrl Pts',(-38.5016942198358,0.164047634942325,
4.15461433304697));
#26993=CARTESIAN_POINT('Ctrl Pts',(-38.5076755410745,0.687592626235074,
4.10060475917359));
#26994=CARTESIAN_POINT('Ctrl Pts',(-38.5210395565078,1.70490817498503,3.79488758815944));
#26995=CARTESIAN_POINT('Ctrl Pts',(-38.5280414898454,2.18704462559348,3.5390280401939));
#26996=CARTESIAN_POINT('Ctrl Pts',(-38.5416969670434,3.02814092354596,2.85349529517244));
#26997=CARTESIAN_POINT('Ctrl Pts',(-38.547867103372,3.37792837628264,2.42933391002391));
#26998=CARTESIAN_POINT('Ctrl Pts',(-38.5601961270754,3.88417209712161,1.48534513332595));
#26999=CARTESIAN_POINT('Ctrl Pts',(-38.5667741100694,4.04190583936277,0.977768857113072));
#27000=CARTESIAN_POINT('Ctrl Pts',(-38.580514306922,4.16019826172762,-0.0898393663118697));
#27001=CARTESIAN_POINT('Ctrl Pts',(-38.5875529536404,4.11157098037679,-0.640553823867985));
#27002=CARTESIAN_POINT('Ctrl Pts',(-38.6006409460874,3.80769852020947,-1.67203224909574));
#27003=CARTESIAN_POINT('Ctrl Pts',(-38.6062398918612,3.56271849964873,-2.14506326699018));
#27004=CARTESIAN_POINT('Ctrl Pts',(-38.6190522367407,2.90477027887625,-2.97686140441376));
#27005=CARTESIAN_POINT('Ctrl Pts',(-38.6258723825032,2.49647225022286,-3.32671241854949));
#27006=CARTESIAN_POINT('Ctrl Pts',(-38.6396995077155,1.55772831997847,-3.85842079894035));
#27007=CARTESIAN_POINT('Ctrl Pts',(-38.6465702471808,1.03372763497844,-4.03055134652997));
#27008=CARTESIAN_POINT('Ctrl Pts',(-38.6548230212139,0.328042356742512,
-4.11522730771825));
#27009=CARTESIAN_POINT('Ctrl Pts',(-38.6566335954254,0.163937275725416,
-4.12499999999999));
#27010=CARTESIAN_POINT('Ctrl Pts',(-38.6584904640031,-1.23582119034381E-14,
-4.12499999999999));
#27011=CARTESIAN_POINT('Ctrl Pts',(-38.5791154631359,-5.54544126205271E-14,
-4.12499999999999));
#27012=CARTESIAN_POINT('Ctrl Pts',(-38.5777052984279,0.124499150524016,
-4.12499999999999));
#27013=CARTESIAN_POINT('Ctrl Pts',(-38.5763345689061,0.249135344500066,
-4.11936371508453));
#27014=CARTESIAN_POINT('Ctrl Pts',(-38.5686514172062,0.917403659595085,
-4.05860129543216));
#27015=CARTESIAN_POINT('Ctrl Pts',(-38.5618328524111,1.44608084437713,-3.90162976661254));
#27016=CARTESIAN_POINT('Ctrl Pts',(-38.5480104953561,2.40099318624483,-3.39649766423788));
#27017=CARTESIAN_POINT('Ctrl Pts',(-38.5411446346849,2.82019163732253,-3.05736616861612));
#27018=CARTESIAN_POINT('Ctrl Pts',(-38.528222099859,3.50032561853965,-2.24486338919386));
#27019=CARTESIAN_POINT('Ctrl Pts',(-38.522643354713,3.75751718053833,-1.78122293458685));
#27020=CARTESIAN_POINT('Ctrl Pts',(-38.5096991233565,4.09141308629972,-0.759909471639569));
#27021=CARTESIAN_POINT('Ctrl Pts',(-38.5026671363584,4.15612476431192,-0.209152794560566));
#27022=CARTESIAN_POINT('Ctrl Pts',(-38.4888638531382,4.06783773883121,0.864423994213772));
#27023=CARTESIAN_POINT('Ctrl Pts',(-38.4822203542193,3.9238733786363,1.37759136778585));
#27024=CARTESIAN_POINT('Ctrl Pts',(-38.4697714822992,3.44514179888959,2.33188908306655));
#27025=CARTESIAN_POINT('Ctrl Pts',(-38.4638107939175,3.11094493722129,2.76201665332028));
#27026=CARTESIAN_POINT('Ctrl Pts',(-38.4502862636308,2.29387538428945,3.47099423492359));
#27027=CARTESIAN_POINT('Ctrl Pts',(-38.4432656612203,1.81822607978738,3.74215421063642));
#27028=CARTESIAN_POINT('Ctrl Pts',(-38.4297991159506,0.808214524886094,
4.07863262096241));
#27029=CARTESIAN_POINT('Ctrl Pts',(-38.4235994038568,0.285791044091418,
4.14810329170106));
#27030=CARTESIAN_POINT('Ctrl Pts',(-38.411580817241,-0.780819452979407,
4.08706579109104));
#27031=CARTESIAN_POINT('Ctrl Pts',(-38.4048303659324,-1.31438245457892,
3.9479329072716));
#27032=CARTESIAN_POINT('Ctrl Pts',(-38.3910281491536,-2.28719728908359,
3.47441347868357));
#27033=CARTESIAN_POINT('Ctrl Pts',(-38.3841155735743,-2.71876148407847,
3.14819940317982));
#27034=CARTESIAN_POINT('Ctrl Pts',(-38.3710678815349,-3.4245630366514,2.35836231288253));
#27035=CARTESIAN_POINT('Ctrl Pts',(-38.3654566966874,-3.69584460745119,
1.90531768684261));
#27036=CARTESIAN_POINT('Ctrl Pts',(-38.3526822593364,-4.06402646341166,
0.896050910667726));
#27037=CARTESIAN_POINT('Ctrl Pts',(-38.3456650689886,-4.14724396373961,
0.345802138784072));
#27038=CARTESIAN_POINT('Ctrl Pts',(-38.3318025171984,-4.09366352410783,
-0.733609595231798));
#27039=CARTESIAN_POINT('Ctrl Pts',(-38.3250897978148,-3.96571863384391,
-1.25273559605927));
#27040=CARTESIAN_POINT('Ctrl Pts',(-38.312507079564,-3.51843465170034,-2.21857153579474));
#27041=CARTESIAN_POINT('Ctrl Pts',(-38.3067294990485,-3.20159152013847,
-2.65542024677681));
#27042=CARTESIAN_POINT('Ctrl Pts',(-38.2933589300789,-2.41190819510755,
-3.39033953816649));
#27043=CARTESIAN_POINT('Ctrl Pts',(-38.2863247626057,-1.94414638530157,
-3.67858612594586));
#27044=CARTESIAN_POINT('Ctrl Pts',(-38.2731805804295,-0.974777894902451,
-4.03797668959702));
#27045=CARTESIAN_POINT('Ctrl Pts',(-38.2671563241853,-0.489185759583953,
-4.12499999999983));
#27046=CARTESIAN_POINT('Ctrl Pts',(-38.261615463136,-1.3759826611448E-12,
-4.12499999999999));
#27047=CARTESIAN_POINT('Origin',(-44.,0.,0.));
#27048=CARTESIAN_POINT('',(-37.9441154631359,-4.83767438976534E-15,-4.12499999999999));
#27049=CARTESIAN_POINT('',(-38.0234904636412,1.59756785521265E-8,-4.12499999999999));
#27050=CARTESIAN_POINT('',(-44.,-5.05166804648282E-16,-4.12499999999999));
#27051=CARTESIAN_POINT('Ctrl Pts',(-38.0234904638221,1.59777359460301E-8,
-4.12499999999999));
#27052=CARTESIAN_POINT('Ctrl Pts',(-38.0237043202452,-0.0188807168282395,
-4.12500000007312));
#27053=CARTESIAN_POINT('Ctrl Pts',(-38.0239190251932,-0.037767437987376,
-4.12487037046446));
#27054=CARTESIAN_POINT('Ctrl Pts',(-38.030132982982,-0.582400873088368,
-4.11738886468603));
#27055=CARTESIAN_POINT('Ctrl Pts',(-38.036666147453,-1.10194175114423,-4.00971289103375));
#27056=CARTESIAN_POINT('Ctrl Pts',(-38.0503600124608,-2.0915695050058,-3.59715313532195));
#27057=CARTESIAN_POINT('Ctrl Pts',(-38.0573998806197,-2.54913449809062,
-3.28878256199403));
#27058=CARTESIAN_POINT('Ctrl Pts',(-38.0705785109338,-3.30574968149235,
-2.52354132989884));
#27059=CARTESIAN_POINT('Ctrl Pts',(-38.0762139412877,-3.60216899750856,
-2.07860995930911));
#27060=CARTESIAN_POINT('Ctrl Pts',(-38.0889546415996,-4.01127620085621,
-1.09911821341874));
#27061=CARTESIAN_POINT('Ctrl Pts',(-38.0957429434606,-4.11941725962378,
-0.573405193795346));
#27062=CARTESIAN_POINT('Ctrl Pts',(-38.109567093331,-4.13030764530197,0.504501949583931));
#27063=CARTESIAN_POINT('Ctrl Pts',(-38.1164680692199,-4.02729010836241,
1.04637739463638));
#27064=CARTESIAN_POINT('Ctrl Pts',(-38.1289758842185,-3.62528197375484,
2.03602879459263));
#27065=CARTESIAN_POINT('Ctrl Pts',(-38.1346887608154,-3.33882262695728,
2.47797306655773));
#27066=CARTESIAN_POINT('Ctrl Pts',(-38.1478682160114,-2.6053850947198,3.24296611051257));
#27067=CARTESIAN_POINT('Ctrl Pts',(-38.1548233679752,-2.16083706612372,
3.55466482608879));
#27068=CARTESIAN_POINT('Ctrl Pts',(-38.1685876557074,-1.16965371430349,
3.99320900259259));
#27069=CARTESIAN_POINT('Ctrl Pts',(-38.1751626900788,-0.631358802437693,
4.11280596691297));
#27070=CARTESIAN_POINT('Ctrl Pts',(-38.1871468020538,0.438465805498592,
4.134968133176));
#27071=CARTESIAN_POINT('Ctrl Pts',(-38.1935866920777,0.95966217178111,4.04589330651222));
#27072=CARTESIAN_POINT('Ctrl Pts',(-38.207177364227,1.95982939445767,3.67028992410267));
#27073=CARTESIAN_POINT('Ctrl Pts',(-38.2142126717834,2.42655689980747,3.37990878902027));
#27074=CARTESIAN_POINT('Ctrl Pts',(-38.2275634299127,3.21277574063565,2.6417632140657));
#27075=CARTESIAN_POINT('Ctrl Pts',(-38.2333220673957,3.52745304345701,2.20406743014782));
#27076=CARTESIAN_POINT('Ctrl Pts',(-38.2459215193518,3.97074923950501,1.23678700030555));
#27077=CARTESIAN_POINT('Ctrl Pts',(-38.2526425728528,4.09664290430123,0.716939305680258));
#27078=CARTESIAN_POINT('Ctrl Pts',(-38.2665116457084,4.14579456083928,-0.363135729722965));
#27079=CARTESIAN_POINT('Ctrl Pts',(-38.2735264080823,4.06022308534345,-0.913277321608179));
#27080=CARTESIAN_POINT('Ctrl Pts',(-38.2862789110268,3.68769584072957,-1.92098495243211));
#27081=CARTESIAN_POINT('Ctrl Pts',(-38.2918985471915,3.4146152650931,-2.37269647451847));
#27082=CARTESIAN_POINT('Ctrl Pts',(-38.3049620365485,2.70553536602887,-3.15961094780644));
#27083=CARTESIAN_POINT('Ctrl Pts',(-38.3118800875951,2.27241232352458,-3.48413580392644));
#27084=CARTESIAN_POINT('Ctrl Pts',(-38.3256785830878,1.2973759659784,-3.95355263983835));
#27085=CARTESIAN_POINT('Ctrl Pts',(-38.3324197327732,0.763230661045134,
-4.09038534611251));
#27086=CARTESIAN_POINT('Ctrl Pts',(-38.339364533471,0.145294655553673,-4.12308259222839));
#27087=CARTESIAN_POINT('Ctrl Pts',(-38.3401679774318,0.0726148363152235,
-4.12499999999999));
#27088=CARTESIAN_POINT('Ctrl Pts',(-38.3409904640031,3.27860210979314E-14,
-4.12499999999999));
#27089=CARTESIAN_POINT('Ctrl Pts',(-38.261615463136,-1.38636031551329E-12,
-4.12499999999999));
#27090=CARTESIAN_POINT('Ctrl Pts',(-38.2612299027003,0.0340399574915664,
-4.125));
#27091=CARTESIAN_POINT('Ctrl Pts',(-38.260846682765,0.0680973155369406,
-4.12457864916165));
#27092=CARTESIAN_POINT('Ctrl Pts',(-38.2543646522353,0.648015297153039,
-4.11021134172938));
#27093=CARTESIAN_POINT('Ctrl Pts',(-38.2477546034083,1.18579871497768,-3.98844139822242));
#27094=CARTESIAN_POINT('Ctrl Pts',(-38.2339854518078,2.17498861886444,-3.54599154814852));
#27095=CARTESIAN_POINT('Ctrl Pts',(-38.2270346006617,2.61812006051472,-3.23265848310332));
#27096=CARTESIAN_POINT('Ctrl Pts',(-38.2138695437158,3.34850409647604,-2.46489685055937));
#27097=CARTESIAN_POINT('Ctrl Pts',(-38.2081712912561,3.63328432239769,-2.02174111422272));
#27098=CARTESIAN_POINT('Ctrl Pts',(-38.1956400875167,4.03140816708781,-1.03040102852718));
#27099=CARTESIAN_POINT('Ctrl Pts',(-38.1887328847935,4.13227712503136,-0.488114918740732));
#27100=CARTESIAN_POINT('Ctrl Pts',(-38.1749099932757,4.11711234980687,0.589544807818989));
#27101=CARTESIAN_POINT('Ctrl Pts',(-38.1681288515778,4.00696696566288,1.11462934019106));
#27102=CARTESIAN_POINT('Ctrl Pts',(-38.1554037880281,3.59402685237509,2.09276756622477));
#27103=CARTESIAN_POINT('Ctrl Pts',(-38.1497580216216,3.29558782142648,2.53688925902393));
#27104=CARTESIAN_POINT('Ctrl Pts',(-38.1365599064696,2.53566351202438,3.29914226321505));
#27105=CARTESIAN_POINT('Ctrl Pts',(-38.1295200916333,2.07704592276241,3.60552433718027));
#27106=CARTESIAN_POINT('Ctrl Pts',(-38.1158368839312,1.08617970980033,4.01398531250382));
#27107=CARTESIAN_POINT('Ctrl Pts',(-38.1093137281357,0.5664222643215,4.11959210542275));
#27108=CARTESIAN_POINT('Ctrl Pts',(-38.0970810830802,-0.507902906672018,
4.13023294250604));
#27109=CARTESIAN_POINT('Ctrl Pts',(-38.0907132693152,-1.05227289152958,
4.02610542998951));
#27110=CARTESIAN_POINT('Ctrl Pts',(-38.0769573558672,-2.05953550630973,
3.61452533619776));
#27111=CARTESIAN_POINT('Ctrl Pts',(-38.0699747351249,-2.51395801148782,
3.31458834453322));
#27112=CARTESIAN_POINT('Ctrl Pts',(-38.0566947382491,-3.26897144918954,
2.56933397632723));
#27113=CARTESIAN_POINT('Ctrl Pts',(-38.0508546849896,-3.5673225554335,2.13584965034781));
#27114=CARTESIAN_POINT('Ctrl Pts',(-38.0385130804182,-3.99655631436128,
1.15821196910055));
#27115=CARTESIAN_POINT('Ctrl Pts',(-38.0316590036003,-4.11462839855131,
0.619468947952946));
#27116=CARTESIAN_POINT('Ctrl Pts',(-38.0178321816844,-4.13383456908287,
-0.459697610602726));
#27117=CARTESIAN_POINT('Ctrl Pts',(-38.0109962994696,-4.03987288087036,
-0.989617065277204));
#27118=CARTESIAN_POINT('Ctrl Pts',(-37.9981471168202,-3.65770806718893,
-1.97851131193549));
#27119=CARTESIAN_POINT('Ctrl Pts',(-37.9925598467427,-3.37529914618813,
-2.4291338025587));
#27120=CARTESIAN_POINT('Ctrl Pts',(-37.979519328704,-2.64186452265411,-3.21503866544509));
#27121=CARTESIAN_POINT('Ctrl Pts',(-37.9724822573282,-2.1918677657622,-3.53717863291173));
#27122=CARTESIAN_POINT('Ctrl Pts',(-37.9587198550079,-1.21133133076715,
-3.97821685582181));
#27123=CARTESIAN_POINT('Ctrl Pts',(-37.9521195020808,-0.693525696132982,
-4.10031256189765));
#27124=CARTESIAN_POINT('Ctrl Pts',(-37.9453813564874,-0.111165010097093,
-4.12387746693034));
#27125=CARTESIAN_POINT('Ctrl Pts',(-37.9447447827213,-0.0555607109844483,
-4.12499999999999));
#27126=CARTESIAN_POINT('Ctrl Pts',(-37.9441154631359,3.30485893395059E-14,
-4.12499999999999));
#27127=CARTESIAN_POINT('Origin',(-44.,0.,0.));
#27128=CARTESIAN_POINT('',(-37.6266154631359,1.21767103030497E-14,-4.12499999999999));
#27129=CARTESIAN_POINT('',(-37.7059904640031,7.79577065882059E-16,-4.12499999999999));
#27130=CARTESIAN_POINT('',(-44.,-5.05166804648282E-16,-4.12499999999999));
#27131=CARTESIAN_POINT('Ctrl Pts',(-37.7059904640031,3.11209391590239E-14,
-4.12499999999999));
#27132=CARTESIAN_POINT('Ctrl Pts',(-37.7071719154616,-0.104306753770122,
-4.12499999999999));
#27133=CARTESIAN_POINT('Ctrl Pts',(-37.7083785054262,-0.208729338301771,
-4.12104375753856));
#27134=CARTESIAN_POINT('Ctrl Pts',(-37.7158245362891,-0.840548388610822,
-4.07295667726032));
#27135=CARTESIAN_POINT('Ctrl Pts',(-37.7225071923448,-1.35543391274962,
-3.93170313299287));
#27136=CARTESIAN_POINT('Ctrl Pts',(-37.7363450634051,-2.32263846728263,
-3.45306018718478));
#27137=CARTESIAN_POINT('Ctrl Pts',(-37.7433697948314,-2.76194610528908,
-3.11286588078123));
#27138=CARTESIAN_POINT('Ctrl Pts',(-37.7562205470214,-3.4642312144117,-2.29988670946835));
#27139=CARTESIAN_POINT('Ctrl Pts',(-37.7618098369706,-3.72815632765471,
-1.84152882982802));
#27140=CARTESIAN_POINT('Ctrl Pts',(-37.7748019154436,-4.07382258539091,
-0.840214112469761));
#27141=CARTESIAN_POINT('Ctrl Pts',(-37.7816944504239,-4.14835405482069,
-0.305197208511262));
#27142=CARTESIAN_POINT('Ctrl Pts',(-37.7955076304459,-4.08830380309599,
0.774331585360137));
#27143=CARTESIAN_POINT('Ctrl Pts',(-37.8022895529962,-3.95000804636215,
1.30815278024656));
#27144=CARTESIAN_POINT('Ctrl Pts',(-37.8144012239025,-3.48410861140897,
2.2691359668022));
#27145=CARTESIAN_POINT('Ctrl Pts',(-37.8204824693978,-3.16936772350144,
2.69130321045133));
#27146=CARTESIAN_POINT('Ctrl Pts',(-37.8338964591907,-2.38482443113829,
3.40901070340842));
#27147=CARTESIAN_POINT('Ctrl Pts',(-37.8409081934389,-1.91729343823775,
3.69225241593301));
#27148=CARTESIAN_POINT('Ctrl Pts',(-37.8545010384649,-0.898986506707305,
4.06217004115416));
#27149=CARTESIAN_POINT('Ctrl Pts',(-37.8605644897187,-0.358038443827645,
4.14502149368244));
#27150=CARTESIAN_POINT('Ctrl Pts',(-37.872951594501,0.710296533020388,4.09746768838102));
#27151=CARTESIAN_POINT('Ctrl Pts',(-37.8795617176277,1.22780524901194,3.97319128026447));
#27152=CARTESIAN_POINT('Ctrl Pts',(-37.8933336100623,2.20689647277595,3.52785923744461));
#27153=CARTESIAN_POINT('Ctrl Pts',(-37.9003697746898,2.65571311685408,3.20365036036623));
#27154=CARTESIAN_POINT('Ctrl Pts',(-37.9133890534834,3.38562313401503,2.41464331803595));
#27155=CARTESIAN_POINT('Ctrl Pts',(-37.9189727139994,3.66592175967749,1.96315157358555));
#27156=CARTESIAN_POINT('Ctrl Pts',(-37.9318382317976,4.04397461112516,0.972839587999278));
#27157=CARTESIAN_POINT('Ctrl Pts',(-37.9386809484601,4.13575917118188,0.442311017554957));
#27158=CARTESIAN_POINT('Ctrl Pts',(-37.9525072262703,4.11195377324833,-0.636973709161365));
#27159=CARTESIAN_POINT('Ctrl Pts',(-37.9593536664618,3.99159250933317,-1.17520101129804));
#27160=CARTESIAN_POINT('Ctrl Pts',(-37.9716696337007,3.55821552618004,-2.15098365823107));
#27161=CARTESIAN_POINT('Ctrl Pts',(-37.9775328773114,3.25803487894005,-2.58318509027641));
#27162=CARTESIAN_POINT('Ctrl Pts',(-37.9908281067754,2.49971153859421,-3.32538326764968));
#27163=CARTESIAN_POINT('Ctrl Pts',(-37.9978144833221,2.0437958034592,-3.62348308224314));
#27164=CARTESIAN_POINT('Ctrl Pts',(-38.0113139570659,1.0527773045935,-4.02333612530768));
#27165=CARTESIAN_POINT('Ctrl Pts',(-38.017501564914,0.528741675688592,-4.12499999795197));
#27166=CARTESIAN_POINT('Ctrl Pts',(-38.0234904638221,1.59777359460301E-8,
-4.12499999999999));
#27167=CARTESIAN_POINT('Ctrl Pts',(-37.9441154631359,3.30485893395059E-14,
-4.12499999999999));
#27168=CARTESIAN_POINT('Ctrl Pts',(-37.9386082192858,0.486217799373158,
-4.12499999999999));
#27169=CARTESIAN_POINT('Ctrl Pts',(-37.9329560684286,0.969089658383457,
-4.03902823711872));
#27170=CARTESIAN_POINT('Ctrl Pts',(-37.9200428786222,1.93393206262313,-3.68352885891709));
#27171=CARTESIAN_POINT('Ctrl Pts',(-37.9130339975976,2.39997383235154,-3.39832360911064));
#27172=CARTESIAN_POINT('Ctrl Pts',(-37.8996352616012,3.18110574425277,-2.6774006466607));
#27173=CARTESIAN_POINT('Ctrl Pts',(-37.893585808979,3.49394459573158,-2.25394013855885));
#27174=CARTESIAN_POINT('Ctrl Pts',(-37.8814474411251,3.9556418650188,-1.29102132570522));
#27175=CARTESIAN_POINT('Ctrl Pts',(-37.874656726913,4.09162469796749,-0.756595147888483));
#27176=CARTESIAN_POINT('Ctrl Pts',(-37.8608409692424,4.1469792361025,0.322970725341458));
#27177=CARTESIAN_POINT('Ctrl Pts',(-37.8539544842789,4.0702029115977,0.857437334283189));
#27178=CARTESIAN_POINT('Ctrl Pts',(-37.8409785885251,3.72034108541746,1.85734328266859));
#27179=CARTESIAN_POINT('Ctrl Pts',(-37.8353934033817,3.45431900223811,2.31480906659922));
#27180=CARTESIAN_POINT('Ctrl Pts',(-37.8225207064847,2.7484693577872,3.12472810048405));
#27181=CARTESIAN_POINT('Ctrl Pts',(-37.8154940725128,2.30790932846725,3.46288290694763));
#27182=CARTESIAN_POINT('Ctrl Pts',(-37.8016638830572,1.33911603179397,3.93726238194202));
#27183=CARTESIAN_POINT('Ctrl Pts',(-37.7949901848288,0.823862854142894,
4.07633708048196));
#27184=CARTESIAN_POINT('Ctrl Pts',(-37.7824839641823,-0.239538409426059,
4.15294827975522));
#27185=CARTESIAN_POINT('Ctrl Pts',(-37.7766085001214,-0.777902064061751,
4.08646922985062));
#27186=CARTESIAN_POINT('Ctrl Pts',(-37.7631489523892,-1.80425003631519,
3.74902840221135));
#27187=CARTESIAN_POINT('Ctrl Pts',(-37.7561215790285,-2.28160006467931,
3.47919986955755));
#27188=CARTESIAN_POINT('Ctrl Pts',(-37.7426068202433,-3.08904281714978,
2.78331574416901));
#27189=CARTESIAN_POINT('Ctrl Pts',(-37.7362858709818,-3.41662368201338,
2.36974547436992));
#27190=CARTESIAN_POINT('Ctrl Pts',(-37.7243542611244,-3.91051726854039,
1.42182952121731));
#27191=CARTESIAN_POINT('Ctrl Pts',(-37.7176343347561,-4.06417530920901,
0.892307582580152));
#27192=CARTESIAN_POINT('Ctrl Pts',(-37.7038450797497,-4.15557849765509,
-0.18644992224989));
#27193=CARTESIAN_POINT('Ctrl Pts',(-37.6969152330419,-4.09610964510732,
-0.72490314925878));
#27194=CARTESIAN_POINT('Ctrl Pts',(-37.6838166935475,-3.77847646188367,
-1.73550079173319));
#27195=CARTESIAN_POINT('Ctrl Pts',(-37.6781747173947,-3.52838754139827,
-2.19984681245613));
#27196=CARTESIAN_POINT('Ctrl Pts',(-37.6654712927782,-2.84980298586446,
-3.0329374391025));
#27197=CARTESIAN_POINT('Ctrl Pts',(-37.6584623742839,-2.41900734548028,
-3.38651484829051));
#27198=CARTESIAN_POINT('Ctrl Pts',(-37.6445796147704,-1.46276901221373,
-3.89323569776352));
#27199=CARTESIAN_POINT('Ctrl Pts',(-37.6378403980949,-0.950543086530867,
-4.048882749067));
#27200=CARTESIAN_POINT('Ctrl Pts',(-37.6298547851239,-0.2821464109366,-4.11777148580024));
#27201=CARTESIAN_POINT('Ctrl Pts',(-37.6282124466366,-0.140992813189271,
-4.12499999999999));
#27202=CARTESIAN_POINT('Ctrl Pts',(-37.6266154631359,3.37577188425087E-14,
-4.12499999999999));
#27203=CARTESIAN_POINT('Origin',(-44.,0.,0.));
#27204=CARTESIAN_POINT('',(-37.3091154631359,-1.27599396641169E-14,-4.12499999999999));
#27205=CARTESIAN_POINT('',(-37.3884904640031,2.95665502823295E-15,-4.12499999999999));
#27206=CARTESIAN_POINT('',(-44.,-5.05166804648282E-16,-4.12499999999999));
#27207=CARTESIAN_POINT('Ctrl Pts',(-37.3884904640031,4.18415302405606E-14,
-4.12499999999999));
#27208=CARTESIAN_POINT('Ctrl Pts',(-37.3906677996739,-0.192230340109688,
-4.12499999999999));
#27209=CARTESIAN_POINT('Ctrl Pts',(-37.3929279773324,-0.384630026067662,
-4.11156311004193));
#27210=CARTESIAN_POINT('Ctrl Pts',(-37.401674325966,-1.10297693745552,-4.01030180346646));
#27211=CARTESIAN_POINT('Ctrl Pts',(-37.4084846352612,-1.61082675698653,
-3.8346200178468));
#27212=CARTESIAN_POINT('Ctrl Pts',(-37.4223113259809,-2.54358162617868,
-3.29304306127044));
#27213=CARTESIAN_POINT('Ctrl Pts',(-37.4291918755208,-2.95678364777868,
-2.9276917129905));
#27214=CARTESIAN_POINT('Ctrl Pts',(-37.4416252892661,-3.60205440330305,
-2.07678052243481));
#27215=CARTESIAN_POINT('Ctrl Pts',(-37.447390089747,-3.83558733235126,-1.60501985013439));
#27216=CARTESIAN_POINT('Ctrl Pts',(-37.4606149346607,-4.11889089965305,
-0.583371534056672));
#27217=CARTESIAN_POINT('Ctrl Pts',(-37.467583052079,-4.15979311380797,-0.0412848199325075));
#27218=CARTESIAN_POINT('Ctrl Pts',(-37.4814017227819,-4.02940642868627,
1.04112845091884));
#27219=CARTESIAN_POINT('Ctrl Pts',(-37.4879109192177,-3.85417530706214,
1.57015298071717));
#27220=CARTESIAN_POINT('Ctrl Pts',(-37.5000810653711,-3.31937920069351,
2.5045662885685));
#27221=CARTESIAN_POINT('Ctrl Pts',(-37.50656775067,-2.9740844161738,2.9061905084859));
#27222=CARTESIAN_POINT('Ctrl Pts',(-37.5202112442221,-2.13546138659101,
3.57111304049778));
#27223=CARTESIAN_POINT('Ctrl Pts',(-37.5272499413056,-1.64514211144103,
3.82185219420493));
#27224=CARTESIAN_POINT('Ctrl Pts',(-37.5405169107563,-0.608441543413077,
4.11439654700987));
#27225=CARTESIAN_POINT('Ctrl Pts',(-37.5462064780509,-0.0734792402402831,
4.15849241465475));
#27226=CARTESIAN_POINT('Ctrl Pts',(-37.5588755836663,0.982700030052533,
4.0412526122613));
#27227=CARTESIAN_POINT('Ctrl Pts',(-37.5656305098631,1.4940702052209,3.88138766260919));
#27228=CARTESIAN_POINT('Ctrl Pts',(-37.5794471667734,2.44163648718631,3.36933297200938));
#27229=CARTESIAN_POINT('Ctrl Pts',(-37.5863755880347,2.86585992415229,3.01676109756999));
#27230=CARTESIAN_POINT('Ctrl Pts',(-37.5989893459416,3.53739310751232,2.18529735335871));
#27231=CARTESIAN_POINT('Ctrl Pts',(-37.6046425622615,3.78549972323502,1.72007830282347));
#27232=CARTESIAN_POINT('Ctrl Pts',(-37.6177562976578,4.09906719353762,0.708153398053445));
#27233=CARTESIAN_POINT('Ctrl Pts',(-37.6246911044208,4.15634329523982,0.169236712848066));
#27234=CARTESIAN_POINT('Ctrl Pts',(-37.6384759248595,4.06039816119926,-0.909333502735539));
#27235=CARTESIAN_POINT('Ctrl Pts',(-37.6451863953515,3.90452636076152,-1.43819518664312));
#27236=CARTESIAN_POINT('Ctrl Pts',(-37.6570916539256,3.40658457875049,-2.38419709865056));
#27237=CARTESIAN_POINT('Ctrl Pts',(-37.6634513160399,3.07712163443936,-2.79652624400761));
#27238=CARTESIAN_POINT('Ctrl Pts',(-37.6769805095977,2.26634299259602,-3.48919522994443));
#27239=CARTESIAN_POINT('Ctrl Pts',(-37.6840096457051,1.78758898584713,-3.75703623297596));
#27240=CARTESIAN_POINT('Ctrl Pts',(-37.69614742799,0.859635779401281,-4.0575058335108));
#27241=CARTESIAN_POINT('Ctrl Pts',(-37.7011108218793,0.430808752928153,
-4.12499999999999));
#27242=CARTESIAN_POINT('Ctrl Pts',(-37.7059904640031,3.27860210979314E-14,
-4.12499999999999));
#27243=CARTESIAN_POINT('Ctrl Pts',(-37.6266154631359,3.30485893395059E-14,
-4.12499999999999));
#27244=CARTESIAN_POINT('Ctrl Pts',(-37.6221989279767,0.389922448398557,
-4.12499999999999));
#27245=CARTESIAN_POINT('Ctrl Pts',(-37.6177368604089,0.778610707645908,
-4.06970972028326));
#27246=CARTESIAN_POINT('Ctrl Pts',(-37.6061774717959,1.67744214455319,-3.80771903698248));
#27247=CARTESIAN_POINT('Ctrl Pts',(-37.5991400897554,2.16520677060958,-3.55308503701036));
#27248=CARTESIAN_POINT('Ctrl Pts',(-37.5855208910561,2.99763324700018,-2.88181979463759));
#27249=CARTESIAN_POINT('Ctrl Pts',(-37.5790559484525,3.3393912706149,-2.47773399156515));
#27250=CARTESIAN_POINT('Ctrl Pts',(-37.5670063158095,3.86377204801705,-1.54438058168654));
#27251=CARTESIAN_POINT('Ctrl Pts',(-37.5605061416315,4.03407359169118,-1.01986013443005));
#27252=CARTESIAN_POINT('Ctrl Pts',(-37.5467534095254,4.15957777932814,0.0572394073939091));
#27253=CARTESIAN_POINT('Ctrl Pts',(-37.5397891031469,4.11662669254909,0.598957311171912));
#27254=CARTESIAN_POINT('Ctrl Pts',(-37.5265779358719,3.8295442392963,1.61940680611599));
#27255=CARTESIAN_POINT('Ctrl Pts',(-37.5208297206459,3.59420851434151,2.09034623789868));
#27256=CARTESIAN_POINT('Ctrl Pts',(-37.5083737788738,2.94567772194275,2.93886682586154));
#27257=CARTESIAN_POINT('Ctrl Pts',(-37.5014869460186,2.53108990773232,3.30265518170488));
#27258=CARTESIAN_POINT('Ctrl Pts',(-37.4876607917416,1.59645131974599,3.84060030559607));
#27259=CARTESIAN_POINT('Ctrl Pts',(-37.4808570234391,1.08813968038432,4.01432744434325));
#27260=CARTESIAN_POINT('Ctrl Pts',(-37.4680819755915,0.0369768069942605,
4.1585927484698));
#27261=CARTESIAN_POINT('Ctrl Pts',(-37.462466281356,-0.495884696062968,
4.12908705952985));
#27262=CARTESIAN_POINT('Ctrl Pts',(-37.4493308252688,-1.53893880112688,
3.86605651225515));
#27263=CARTESIAN_POINT('Ctrl Pts',(-37.4422912410479,-2.03738512301656,
3.62819285141658));
#27264=CARTESIAN_POINT('Ctrl Pts',(-37.4285746493976,-2.89589644148774,
2.98434527946527));
#27265=CARTESIAN_POINT('Ctrl Pts',(-37.4220197839471,-3.25260783241754,
2.59096193869904));
#27266=CARTESIAN_POINT('Ctrl Pts',(-37.4097317835589,-3.8093108483045,1.67427029362598));
#27267=CARTESIAN_POINT('Ctrl Pts',(-37.4034805956724,-3.99731289323383,
1.15565172979563));
#27268=CARTESIAN_POINT('Ctrl Pts',(-37.3897818306433,-4.15940421165096,
0.0814839838693053));
#27269=CARTESIAN_POINT('Ctrl Pts',(-37.3827876581262,-4.13433674295738,
-0.463187996524866));
#27270=CARTESIAN_POINT('Ctrl Pts',(-37.3694592448157,-3.88018263989796,
-1.49393259741077));
#27271=CARTESIAN_POINT('Ctrl Pts',(-37.3635417973747,-3.66040480140604,
-1.97207483992736));
#27272=CARTESIAN_POINT('Ctrl Pts',(-37.3512821135096,-3.04009209338073,
-2.8410785534224));
#27273=CARTESIAN_POINT('Ctrl Pts',(-37.3444528046473,-2.63765796626467,
-3.21817317843681));
#27274=CARTESIAN_POINT('Ctrl Pts',(-37.3306285945402,-1.7197367339296,-3.78723625854297));
#27275=CARTESIAN_POINT('Ctrl Pts',(-37.3237713357021,-1.21565176041362,
-3.97779436157307));
#27276=CARTESIAN_POINT('Ctrl Pts',(-37.3144537986562,-0.461036086366698,
-4.10568623576393));
#27277=CARTESIAN_POINT('Ctrl Pts',(-37.3117258674995,-0.230464657033585,
-4.12499999999999));
#27278=CARTESIAN_POINT('Ctrl Pts',(-37.3091154631359,-5.72458747072346E-14,
-4.12499999999999));
#27279=CARTESIAN_POINT('Origin',(-44.,0.,0.));
#27280=CARTESIAN_POINT('',(-36.9916154631359,-6.98331048911415E-15,-4.12499999999999));
#27281=CARTESIAN_POINT('',(-37.0709904640031,-1.50158430502744E-15,-4.12499999999999));
#27282=CARTESIAN_POINT('',(-44.,-5.05166804648282E-16,-4.12499999999999));
#27283=CARTESIAN_POINT('Ctrl Pts',(-37.0709904640031,2.24126273096203E-14,
-4.12499999999999));
#27284=CARTESIAN_POINT('Ctrl Pts',(-37.0741641489576,-0.280194986185825,
-4.12499999999999));
#27285=CARTESIAN_POINT('Ctrl Pts',(-37.0775086187982,-0.560288405338992,
-4.09645124016517));
#27286=CARTESIAN_POINT('Ctrl Pts',(-37.0875708944323,-1.36059888724556,
-3.93083971226053));
#27287=CARTESIAN_POINT('Ctrl Pts',(-37.0944813021594,-1.85915471210682,
-3.72105775932517));
#27288=CARTESIAN_POINT('Ctrl Pts',(-37.1082849003488,-2.75658981046722,
-3.11688834223419));
#27289=CARTESIAN_POINT('Ctrl Pts',(-37.1150389453404,-3.14452540889099,
-2.72502303584165));
#27290=CARTESIAN_POINT('Ctrl Pts',(-37.1270679765999,-3.73215915556418,
-1.83285752755093));
#27291=CARTESIAN_POINT('Ctrl Pts',(-37.1332538109737,-3.93401179253985,
-1.34608573887598));
#27292=CARTESIAN_POINT('Ctrl Pts',(-37.1467145081879,-4.1493789780694,-0.303668488579494));
#27293=CARTESIAN_POINT('Ctrl Pts',(-37.1537341990965,-4.15333077001792,
0.243731308968634));
#27294=CARTESIAN_POINT('Ctrl Pts',(-37.1672664587256,-3.94973777493262,
1.30636085895795));
#27295=CARTESIAN_POINT('Ctrl Pts',(-37.1732380847386,-3.74508229813653,
1.81145242736624));
#27296=CARTESIAN_POINT('Ctrl Pts',(-37.1856800465032,-3.15931852012689,
2.70428532402661));
#27297=CARTESIAN_POINT('Ctrl Pts',(-37.1923198543581,-2.78756277088135,
3.08608794801719));
#27298=CARTESIAN_POINT('Ctrl Pts',(-37.2061197479408,-1.903122333998,3.70069422731297));
#27299=CARTESIAN_POINT('Ctrl Pts',(-37.2131522829967,-1.39425855236916,
3.92084951372823));
#27300=CARTESIAN_POINT('Ctrl Pts',(-37.2261050125298,-0.343180026940343,
4.14415866512579));
#27301=CARTESIAN_POINT('Ctrl Pts',(-37.2316837078612,0.187054260758582,
4.15413466165872));
#27302=CARTESIAN_POINT('Ctrl Pts',(-37.2445998403375,1.2311046276491,3.97306647640316));
#27303=CARTESIAN_POINT('Ctrl Pts',(-37.2514631582721,1.7346373170358,3.78046360371346));
#27304=CARTESIAN_POINT('Ctrl Pts',(-37.2652861146008,2.65045053277971,3.20764410291976));
#27305=CARTESIAN_POINT('Ctrl Pts',(-37.2721079053092,3.05137392703989,2.82895654410468));
#27306=CARTESIAN_POINT('Ctrl Pts',(-37.2843433905178,3.66823469864112,1.95747871483541));
#27307=CARTESIAN_POINT('Ctrl Pts',(-37.2902855230812,3.88611550536358,1.47844008591746));
#27308=CARTESIAN_POINT('Ctrl Pts',(-37.3036280948907,4.13620649609111,0.44644923125366));
#27309=CARTESIAN_POINT('Ctrl Pts',(-37.3106254296513,4.15906352642556,-0.0985465952050307));
#27310=CARTESIAN_POINT('Ctrl Pts',(-37.3243071099761,3.99258790290023,-1.17153483285406));
#27311=CARTESIAN_POINT('Ctrl Pts',(-37.3305255755067,3.8028239865781,-1.68871883264315));
#27312=CARTESIAN_POINT('Ctrl Pts',(-37.3428298566585,3.24307198872039,-2.60292603704322));
#27313=CARTESIAN_POINT('Ctrl Pts',(-37.3493939366953,2.88477608020006,-2.99512911363186));
#27314=CARTESIAN_POINT('Ctrl Pts',(-37.3631200144422,2.02351857378712,-3.63597730023228));
#27315=CARTESIAN_POINT('Ctrl Pts',(-37.3701593059518,1.52395907130064,-3.87201644098539));
#27316=CARTESIAN_POINT('Ctrl Pts',(-37.3809217526081,0.667410969169671,
-4.08444198854481));
#27317=CARTESIAN_POINT('Ctrl Pts',(-37.3847077705848,0.333962490054018,
-4.12499999999999));
#27318=CARTESIAN_POINT('Ctrl Pts',(-37.3884904640031,3.27860210979314E-14,
-4.12499999999999));
#27319=CARTESIAN_POINT('Ctrl Pts',(-37.3091154631359,-5.54544126205271E-14,
-4.12499999999999));
#27320=CARTESIAN_POINT('Ctrl Pts',(-37.3057961344788,0.293053425445313,
-4.125));
#27321=CARTESIAN_POINT('Ctrl Pts',(-37.302496572808,0.585932270930643,-4.09377041876538));
#27322=CARTESIAN_POINT('Ctrl Pts',(-37.2923184130573,1.40993297946147,-3.91520855680477));
#27323=CARTESIAN_POINT('Ctrl Pts',(-37.2852846637679,1.91770377245598,-3.69312550545327));
#27324=CARTESIAN_POINT('Ctrl Pts',(-37.2714929077765,2.79939846988331,-3.07532218924127));
#27325=CARTESIAN_POINT('Ctrl Pts',(-37.26486186999,3.1695519937379,-2.6922455727142));
#27326=CARTESIAN_POINT('Ctrl Pts',(-37.2524362455398,3.75220749517648,-1.79684166298536));
#27327=CARTESIAN_POINT('Ctrl Pts',(-37.246438196426,3.95509588538512,-1.29031930269742));
#27328=CARTESIAN_POINT('Ctrl Pts',(-37.2328877493134,4.15428070878072,-0.226425060803106));
#27329=CARTESIAN_POINT('Ctrl Pts',(-37.225870294532,4.14806623944732,0.320721303783965));
#27330=CARTESIAN_POINT('Ctrl Pts',(-37.2124234556353,3.92854411626132,1.36191250792841));
#27331=CARTESIAN_POINT('Ctrl Pts',(-37.2062698062463,3.72479007920702,1.84775199830548));
#27332=CARTESIAN_POINT('Ctrl Pts',(-37.1942161120231,3.13368508465123,2.73748416652482));
#27333=CARTESIAN_POINT('Ctrl Pts',(-37.18745364341,2.74418912893683,3.12781355623797));
#27334=CARTESIAN_POINT('Ctrl Pts',(-37.1736469341447,1.84452264352381,3.7283029189356));
#27335=CARTESIAN_POINT('Ctrl Pts',(-37.1667417260539,1.34534790700189,3.93605750193924));
#27336=CARTESIAN_POINT('Ctrl Pts',(-37.1537148623995,0.307264370469522,
4.14673386817001));
#27337=CARTESIAN_POINT('Ctrl Pts',(-37.1481133025172,-0.2210657191477,4.15222126708393));
#27338=CARTESIAN_POINT('Ctrl Pts',(-37.1353101195756,-1.27811474097495,
3.96046567143204));
#27339=CARTESIAN_POINT('Ctrl Pts',(-37.1282899220348,-1.79481368830906,
3.75466415770538));
#27340=CARTESIAN_POINT('Ctrl Pts',(-37.1144363003646,-2.69913083967334,
3.16396370377404));
#27341=CARTESIAN_POINT('Ctrl Pts',(-37.1077347087709,-3.08255434702908,
2.79174481769875));
#27342=CARTESIAN_POINT('Ctrl Pts',(-37.095174106695,-3.6910726054665,1.91787434655503));
#27343=CARTESIAN_POINT('Ctrl Pts',(-37.0893701180906,-3.9085740653729,1.42313422703085));
#27344=CARTESIAN_POINT('Ctrl Pts',(-37.0759735564863,-4.14421102863299,
0.369970159798663));
#27345=CARTESIAN_POINT('Ctrl Pts',(-37.0689410874436,-4.15683990406862,
-0.179005345339644));
#27346=CARTESIAN_POINT('Ctrl Pts',(-37.0553814777069,-3.97193906272694,
-1.2302017074355));
#27347=CARTESIAN_POINT('Ctrl Pts',(-37.0489683455837,-3.78391418135595,
-1.72386178107584));
#27348=CARTESIAN_POINT('Ctrl Pts',(-37.0370537589836,-3.22150191021418,
-2.63356290217202));
#27349=CARTESIAN_POINT('Ctrl Pts',(-37.0303963268061,-2.84501717177573,
-3.03638425298011));
#27350=CARTESIAN_POINT('Ctrl Pts',(-37.0166210877952,-1.96412316641114,
-3.66695408089926));
#27351=CARTESIAN_POINT('Ctrl Pts',(-37.0096760739643,-1.47028239282131,
-3.89134987815664));
#27352=CARTESIAN_POINT('Ctrl Pts',(-36.9990436040111,-0.636218269325341,
-4.0881571656051));
#27353=CARTESIAN_POINT('Ctrl Pts',(-36.9952207715431,-0.318301707262144,
-4.12499999999999));
#27354=CARTESIAN_POINT('Ctrl Pts',(-36.9916154631359,3.06699110552699E-14,
-4.12499999999999));
#27355=CARTESIAN_POINT('Origin',(-44.,0.,0.));
#27356=CARTESIAN_POINT('',(-36.6741154631359,1.03986187401735E-14,-4.12499999999999));
#27357=CARTESIAN_POINT('',(-36.7534904640031,-3.56666810882749E-16,-4.12499999999999));
#27358=CARTESIAN_POINT('',(-44.,-5.05166804648282E-16,-4.12499999999999));
#27359=CARTESIAN_POINT('Ctrl Pts',(-36.7534904640031,2.82412981889024E-14,
-4.12499999999999));
#27360=CARTESIAN_POINT('Ctrl Pts',(-36.7576415599671,-0.366487629658998,
-4.12499999999999));
#27361=CARTESIAN_POINT('Ctrl Pts',(-36.7620762393622,-0.732041526592343,
-4.07615668580182));
#27362=CARTESIAN_POINT('Ctrl Pts',(-36.7734266674402,-1.60705638319277,
-3.83715416268648));
#27363=CARTESIAN_POINT('Ctrl Pts',(-36.7804077774656,-2.09434991444426,
-3.59445125081873));
#27364=CARTESIAN_POINT('Ctrl Pts',(-36.7941706433496,-2.9557531315232,-2.92927906028107));
#27365=CARTESIAN_POINT('Ctrl Pts',(-36.8005534185697,-3.31900785527471,
-2.51024406353054));
#27366=CARTESIAN_POINT('Ctrl Pts',(-36.8127792310965,-3.8484799759449,-1.57511694023483));
#27367=CARTESIAN_POINT('Ctrl Pts',(-36.8192984335145,-4.01764523711922,
-1.07252476234264));
#27368=CARTESIAN_POINT('Ctrl Pts',(-36.8329774021165,-4.16097543710129,
-0.0105666975561747));
#27369=CARTESIAN_POINT('Ctrl Pts',(-36.840017164917,-4.12583163241094,0.539763961332355));
#27370=CARTESIAN_POINT('Ctrl Pts',(-36.8532229045633,-3.84732929524882,
1.5795407558575));
#27371=CARTESIAN_POINT('Ctrl Pts',(-36.8588729602128,-3.61259971164264,
2.06058580728881));
#27372=CARTESIAN_POINT('Ctrl Pts',(-36.87159188163,-2.9731886495747,2.90830672082235));
#27373=CARTESIAN_POINT('Ctrl Pts',(-36.8783701907586,-2.57413217337487,
3.26679301273284));
#27374=CARTESIAN_POINT('Ctrl Pts',(-36.8921925295395,-1.649359153071,3.82015542390103));
#27375=CARTESIAN_POINT('Ctrl Pts',(-36.8991021422894,-1.12957504885575,
4.00475229120779));
#27376=CARTESIAN_POINT('Ctrl Pts',(-36.9116424946604,-0.0721770441526228,
4.1572862110603));
#27377=CARTESIAN_POINT('Ctrl Pts',(-36.9173352496109,0.454080222469922,
4.13304406660709));
#27378=CARTESIAN_POINT('Ctrl Pts',(-36.9304946576446,1.48451292117278,3.88597041916154));
#27379=CARTESIAN_POINT('Ctrl Pts',(-36.9374437971501,1.97770750081534,3.65967426590964));
#27380=CARTESIAN_POINT('Ctrl Pts',(-36.951214792953,2.85640483962125,3.02567766666973));
#27381=CARTESIAN_POINT('Ctrl Pts',(-36.9578387518307,3.23138713958174,2.62142868411158));
#27382=CARTESIAN_POINT('Ctrl Pts',(-36.9697812782337,3.79048149629175,1.70943238667739));
#27383=CARTESIAN_POINT('Ctrl Pts',(-36.9762051847253,3.97668136035649,1.21486817836494));
#27384=CARTESIAN_POINT('Ctrl Pts',(-36.9897773735142,4.1575446739385,0.162549653208822));
#27385=CARTESIAN_POINT('Ctrl Pts',(-36.9968110603857,4.14272189801142,-0.386597455608169));
#27386=CARTESIAN_POINT('Ctrl Pts',(-37.0101893544228,3.90287712781141,-1.43848358748678));
#27387=CARTESIAN_POINT('Ctrl Pts',(-37.01597459825,3.68368772343865,-1.93187128553373));
#27388=CARTESIAN_POINT('Ctrl Pts',(-37.028550762786,3.07216024767993,-2.8032152880964));
#27389=CARTESIAN_POINT('Ctrl Pts',(-37.0352601979701,2.68720264144112,-3.174132919078));
#27390=CARTESIAN_POINT('Ctrl Pts',(-37.0491201402536,1.78028797106041,-3.76160625531938));
#27391=CARTESIAN_POINT('Ctrl Pts',(-37.0561382455587,1.26257554819493,-3.96547809484026));
#27392=CARTESIAN_POINT('Ctrl Pts',(-37.0655724171135,0.481878270195129,
-4.10389697683738));
#27393=CARTESIAN_POINT('Ctrl Pts',(-37.0682618379416,0.240902090955855,
-4.12499999999999));
#27394=CARTESIAN_POINT('Ctrl Pts',(-37.0709904640031,3.27860210979314E-14,
-4.12499999999999));
#27395=CARTESIAN_POINT('Ctrl Pts',(-36.9916154631359,3.30485893395059E-14,
-4.12499999999999));
#27396=CARTESIAN_POINT('Ctrl Pts',(-36.9893305241456,0.201730309719417,
-4.12499999999999));
#27397=CARTESIAN_POINT('Ctrl Pts',(-36.9870917054975,0.403614853428467,
-4.11020203186251));
#27398=CARTESIAN_POINT('Ctrl Pts',(-36.978287832153,1.14435371916495,-4.0005551310462));
#27399=CARTESIAN_POINT('Ctrl Pts',(-36.971372561439,1.66345805077401,-3.81403809622079));
#27400=CARTESIAN_POINT('Ctrl Pts',(-36.9575516705327,2.58602406242228,-3.2573567197015));
#27401=CARTESIAN_POINT('Ctrl Pts',(-36.9507801515451,2.9836343999844,-2.89755497283861));
#27402=CARTESIAN_POINT('Ctrl Pts',(-36.9380758561353,3.62016474349483,-2.04737547667693));
#27403=CARTESIAN_POINT('Ctrl Pts',(-36.932415069113,3.85329630924313,-1.56507123600717));
#27404=CARTESIAN_POINT('Ctrl Pts',(-36.9191912398441,4.12783254379462,-0.524021945356768));
#27405=CARTESIAN_POINT('Ctrl Pts',(-36.9121516713196,4.16087846414009,0.0262203002124799));
#27406=CARTESIAN_POINT('Ctrl Pts',(-36.8984829167639,4.01366219794949,1.08724596219465));
#27407=CARTESIAN_POINT('Ctrl Pts',(-36.8919731779874,3.84272750092134,1.58903818341369));
#27408=CARTESIAN_POINT('Ctrl Pts',(-36.8797636626523,3.30962575391587,2.52276737198302));
#27409=CARTESIAN_POINT('Ctrl Pts',(-36.8733447064144,2.94424120069034,2.94099241861182));
#27410=CARTESIAN_POINT('Ctrl Pts',(-36.8595653478843,2.07966474064219,3.60293510571031));
#27411=CARTESIAN_POINT('Ctrl Pts',(-36.8525879158149,1.59159286110859,3.84356345624947));
#27412=CARTESIAN_POINT('Ctrl Pts',(-36.8393282713374,0.567367275551635,
4.11895460724689));
#27413=CARTESIAN_POINT('Ctrl Pts',(-36.8335175660888,0.0425157025061008,
4.1576289332339));
#27414=CARTESIAN_POINT('Ctrl Pts',(-36.8211418984236,-1.01813030924982,
4.03451853867593));
#27415=CARTESIAN_POINT('Ctrl Pts',(-36.814277838969,-1.5427859224169,3.86441874539541));
#27416=CARTESIAN_POINT('Ctrl Pts',(-36.8004506839492,-2.48374759460356,
3.33625510922713));
#27417=CARTESIAN_POINT('Ctrl Pts',(-36.7936240883164,-2.89352715898268,
2.98782625208009));
#27418=CARTESIAN_POINT('Ctrl Pts',(-36.7807967698813,-3.55446914547999,
2.15861648518414));
#27419=CARTESIAN_POINT('Ctrl Pts',(-36.7752031580768,-3.80110005427536,
1.68686532625811));
#27420=CARTESIAN_POINT('Ctrl Pts',(-36.7621343912782,-4.10904539493212,
0.656744278712707));
#27421=CARTESIAN_POINT('Ctrl Pts',(-36.7550963066766,-4.15984699262744,
0.105997737615902));
#27422=CARTESIAN_POINT('Ctrl Pts',(-36.7413469502353,-4.04560200847876,
-0.962466275870112));
#27423=CARTESIAN_POINT('Ctrl Pts',(-36.7347598186218,-3.88972121826326,
-1.47082085340387));
#27424=CARTESIAN_POINT('Ctrl Pts',(-36.7224143915539,-3.38720824987418,
-2.41621937772741));
#27425=CARTESIAN_POINT('Ctrl Pts',(-36.7162753541536,-3.03955768836155,
-2.8411958316692));
#27426=CARTESIAN_POINT('Ctrl Pts',(-36.7026374066437,-2.20172182822143,
-3.52994987558751));
#27427=CARTESIAN_POINT('Ctrl Pts',(-36.6956325634038,-1.72044144332667,
-3.78790261969301));
#27428=CARTESIAN_POINT('Ctrl Pts',(-36.6836820048752,-0.812559101531468,
-4.06473822366178));
#27429=CARTESIAN_POINT('Ctrl Pts',(-36.6787262751517,-0.407074560825465,
-4.12499999999999));
#27430=CARTESIAN_POINT('Ctrl Pts',(-36.6741154631359,2.99760216648792E-14,
-4.12499999999999));
#27431=CARTESIAN_POINT('Origin',(-44.,0.,0.));
#27432=CARTESIAN_POINT('',(-36.3566154631359,-2.34370863720154E-13,-4.12499999999999));
#27433=CARTESIAN_POINT('',(-36.4359904640031,-7.73000445117183E-16,-4.12499999999999));
#27434=CARTESIAN_POINT('',(-44.,-5.05166804648282E-16,-4.12499999999999));
#27435=CARTESIAN_POINT('Ctrl Pts',(-36.4359904640031,4.01068067645838E-14,
-4.12499999999999));
#27436=CARTESIAN_POINT('Ctrl Pts',(-36.4412017256467,-0.460086431121445,
-4.12499999999999));
#27437=CARTESIAN_POINT('Ctrl Pts',(-36.4468453199935,-0.917411502442056,
-4.04802055218068));
#27438=CARTESIAN_POINT('Ctrl Pts',(-36.4595704341114,-1.86580400053964,
-3.71876346043056));
#27439=CARTESIAN_POINT('Ctrl Pts',(-36.4665970710672,-2.338559030851,-3.44115814893948));
#27440=CARTESIAN_POINT('Ctrl Pts',(-36.4800644861582,-3.14536896278283,
-2.72236864022482));
#27441=CARTESIAN_POINT('Ctrl Pts',(-36.485949637797,-3.47301484091786,-2.28971621973573));
#27442=CARTESIAN_POINT('Ctrl Pts',(-36.4984489844205,-3.9399792698403,-1.3310705459252));
#27443=CARTESIAN_POINT('Ctrl Pts',(-36.5051191044568,-4.07798290471611,
-0.815618564857166));
#27444=CARTESIAN_POINT('Ctrl Pts',(-36.5189461858771,-4.15333093926841,
0.260266329513334));
#27445=CARTESIAN_POINT('Ctrl Pts',(-36.5259735381615,-4.081707850498,0.810902849443812));
#27446=CARTESIAN_POINT('Ctrl Pts',(-36.5388549047641,-3.73497882809028,
1.82776098681841));
#27447=CARTESIAN_POINT('Ctrl Pts',(-36.5444387415108,-3.47253378202807,
2.28741933524712));
#27448=CARTESIAN_POINT('Ctrl Pts',(-36.5574082200477,-2.78283398666363,
3.09151917646995));
#27449=CARTESIAN_POINT('Ctrl Pts',(-36.5642922791827,-2.35899467458484,
3.42590079205501));
#27450=CARTESIAN_POINT('Ctrl Pts',(-36.5781089839472,-1.39730663931997,
3.91935804898285));
#27451=CARTESIAN_POINT('Ctrl Pts',(-36.5849031395274,-0.866741587975729,
4.06971768907761));
#27452=CARTESIAN_POINT('Ctrl Pts',(-36.5970520462944,0.197849486082596,
4.15315743767392));
#27453=CARTESIAN_POINT('Ctrl Pts',(-36.6030892187348,0.721064415627516,
4.09486750473588));
#27454=CARTESIAN_POINT('Ctrl Pts',(-36.6164819110651,1.73639216168081,3.78065020492605));
#27455=CARTESIAN_POINT('Ctrl Pts',(-36.6234896276959,2.21678262677909,3.52054665687627));
#27456=CARTESIAN_POINT('Ctrl Pts',(-36.6371094361076,3.05125966565257,2.82848747037175));
#27457=CARTESIAN_POINT('Ctrl Pts',(-36.6432173154938,3.39671597472361,2.40267334681509));
#27458=CARTESIAN_POINT('Ctrl Pts',(-36.655579593977,3.89538494032113,1.45582617198234));
#27459=CARTESIAN_POINT('Ctrl Pts',(-36.6621760659865,4.04935176872739,0.946676204005937));
#27460=CARTESIAN_POINT('Ctrl Pts',(-36.6759346628,4.15941921450689,-0.122654443879365));
#27461=CARTESIAN_POINT('Ctrl Pts',(-36.6829720567077,4.10637495129219,-0.673425426266464));
#27462=CARTESIAN_POINT('Ctrl Pts',(-36.6960209247928,3.79423362638182,-1.70214089576033));
#27463=CARTESIAN_POINT('Ctrl Pts',(-36.7016098851731,3.54590018167344,-2.17257548776153));
#27464=CARTESIAN_POINT('Ctrl Pts',(-36.7144526217738,2.88186875113404,-2.99910917033283));
#27465=CARTESIAN_POINT('Ctrl Pts',(-36.7212857824561,2.47056366634082,-3.34606242349329));
#27466=CARTESIAN_POINT('Ctrl Pts',(-36.7351127493689,1.52732493058807,-3.87055432509153));
#27467=CARTESIAN_POINT('Ctrl Pts',(-36.7419697976526,1.00200118391928,-4.0385535164199));
#27468=CARTESIAN_POINT('Ctrl Pts',(-36.7500661838899,0.30646783432405,-4.11647083312409));
#27469=CARTESIAN_POINT('Ctrl Pts',(-36.7517557524127,0.153152407080955,
-4.12499999999999));
#27470=CARTESIAN_POINT('Ctrl Pts',(-36.7534904640031,3.27860210979314E-14,
-4.12499999999999));
#27471=CARTESIAN_POINT('Ctrl Pts',(-36.6741154631359,3.30485893395059E-14,
-4.12499999999999));
#27472=CARTESIAN_POINT('Ctrl Pts',(-36.6728350826434,0.113040897115812,
-4.12499999999999));
#27473=CARTESIAN_POINT('Ctrl Pts',(-36.6715907614374,0.226204519412501,
-4.12035343434328));
#27474=CARTESIAN_POINT('Ctrl Pts',(-36.6640718447843,0.883457903371157,
-4.0661229212802));
#27475=CARTESIAN_POINT('Ctrl Pts',(-36.6572695230822,1.41340994548097,-3.91358099965638));
#27476=CARTESIAN_POINT('Ctrl Pts',(-36.6434507152114,2.37288000651907,-3.41626486857158));
#27477=CARTESIAN_POINT('Ctrl Pts',(-36.6365725467785,2.79519512461284,-3.08031057313625));
#27478=CARTESIAN_POINT('Ctrl Pts',(-36.6236184889273,3.48174473184279,-2.27343780744332));
#27479=CARTESIAN_POINT('Ctrl Pts',(-36.6180372476477,3.74246021380861,-1.81247249131371));
#27480=CARTESIAN_POINT('Ctrl Pts',(-36.6051351225958,4.08497041813595,-0.794142513631144));
#27481=CARTESIAN_POINT('Ctrl Pts',(-36.5981061277905,4.15431924496963,-0.243457295605664));
#27482=CARTESIAN_POINT('Ctrl Pts',(-36.584286658258,4.07471049198571,0.831685081881199));
#27483=CARTESIAN_POINT('Ctrl Pts',(-36.5776251967898,3.93474251240417,1.34639309586123));
#27484=CARTESIAN_POINT('Ctrl Pts',(-36.5651423937967,3.46390921299336,2.30361325808074));
#27485=CARTESIAN_POINT('Ctrl Pts',(-36.559233334483,3.13411712446255,2.73543703572066));
#27486=CARTESIAN_POINT('Ctrl Pts',(-36.5457470723525,2.32393538993202,3.45101453663675));
#27487=CARTESIAN_POINT('Ctrl Pts',(-36.5387222919395,1.85022107673129,3.7265074323395));
#27488=CARTESIAN_POINT('Ctrl Pts',(-36.5252271503771,0.842349818432827,
4.07175938697056));
#27489=CARTESIAN_POINT('Ctrl Pts',(-36.5189570136296,0.320209919426375,
4.14562707604677));
#27490=CARTESIAN_POINT('Ctrl Pts',(-36.5069898247318,-0.747151170852962,
4.09335153829842));
#27491=CARTESIAN_POINT('Ctrl Pts',(-36.500257283483,-1.28181952513925,3.95862221351396));
#27492=CARTESIAN_POINT('Ctrl Pts',(-36.4864624135428,-2.25887014439116,
3.49296220009469));
#27493=CARTESIAN_POINT('Ctrl Pts',(-36.4795394640567,-2.69341161756348,
3.16998673200341));
#27494=CARTESIAN_POINT('Ctrl Pts',(-36.4664615956043,-3.40548350244653,
2.38574522771969));
#27495=CARTESIAN_POINT('Ctrl Pts',(-36.4608333961484,-3.68020610078538,
1.93524645577792));
#27496=CARTESIAN_POINT('Ctrl Pts',(-36.4481009583221,-4.05669264010034,
0.928965648007552));
#27497=CARTESIAN_POINT('Ctrl Pts',(-36.4410885169197,-4.14441036663435,
0.378930143789663));
#27498=CARTESIAN_POINT('Ctrl Pts',(-36.4272136983967,-4.09929943388298,
-0.701734160415109));
#27499=CARTESIAN_POINT('Ctrl Pts',(-36.4204851386975,-3.97527863817013,
-1.22223274256081));
#27500=CARTESIAN_POINT('Ctrl Pts',(-36.407870485071,-3.53561630564112,-2.19082580413866));
#27501=CARTESIAN_POINT('Ctrl Pts',(-36.4021282742375,-3.22290591681853,
-2.62929272235258));
#27502=CARTESIAN_POINT('Ctrl Pts',(-36.3887956204897,-2.43984218321108,
-3.37036607398834));
#27503=CARTESIAN_POINT('Ctrl Pts',(-36.381759386071,-1.97406363518828,-3.66268583780771));
#27504=CARTESIAN_POINT('Ctrl Pts',(-36.3684548786441,-0.996849952972246,
-4.03394272593325));
#27505=CARTESIAN_POINT('Ctrl Pts',(-36.3622833267925,-0.500398433273007,
-4.12499999999993));
#27506=CARTESIAN_POINT('Ctrl Pts',(-36.3566154631359,-4.95853358373211E-13,
-4.12499999999999));
#27507=CARTESIAN_POINT('Origin',(-44.,0.,0.));
#27508=CARTESIAN_POINT('',(-36.0391154631359,5.89701132001364E-15,-4.12499999999999));
#27509=CARTESIAN_POINT('',(-36.118490463256,3.29787998222272E-8,-4.12499999999999));
#27510=CARTESIAN_POINT('',(-44.,-5.05166804648282E-16,-4.12499999999999));
#27511=CARTESIAN_POINT('',(-36.,2.86773946748161,-2.96507931540595));
#27512=CARTESIAN_POINT('Ctrl Pts',(-36.0391154631359,3.30485893395058E-14,
-4.12499999999999));
#27513=CARTESIAN_POINT('Ctrl Pts',(-36.0337451023778,0.474132807753825,
-4.12499999999999));
#27514=CARTESIAN_POINT('Ctrl Pts',(-36.0282440585244,0.945254618717873,
-4.0432484302357));
#27515=CARTESIAN_POINT('Ctrl Pts',(-36.0186280448279,1.66734526282084,-3.78428978927984));
#27516=CARTESIAN_POINT('Ctrl Pts',(-36.014893553752,1.93096315570308,-3.65681146633632));
#27517=CARTESIAN_POINT('Ctrl Pts',(-36.0074010648044,2.42689448492082,-3.3482992956644));
#27518=CARTESIAN_POINT('Ctrl Pts',(-36.0036641910876,2.65780272692487,-3.16812409516617));
#27519=CARTESIAN_POINT('Ctrl Pts',(-36.,2.86773946747953,-2.96507931540796));
#27520=CARTESIAN_POINT('',(-36.,2.91366312592486,2.91996441564374));
#27521=CARTESIAN_POINT('Origin',(-36.,0.,0.));
#27522=CARTESIAN_POINT('Ctrl Pts',(-36.,2.91366312592486,2.91996441564374));
#27523=CARTESIAN_POINT('Ctrl Pts',(-36.0036344485079,3.12330794772784,2.71077200783361));
#27524=CARTESIAN_POINT('Ctrl Pts',(-36.0071391686434,3.30981666374636,2.4796074816148));
#27525=CARTESIAN_POINT('Ctrl Pts',(-36.0137501146596,3.6292482539912,1.98266554537504));
#27526=CARTESIAN_POINT('Ctrl Pts',(-36.0171520191282,3.76153650954986,1.71850385079139));
#27527=CARTESIAN_POINT('Ctrl Pts',(-36.0272316267131,4.05122661578133,0.9424079233371));
#27528=CARTESIAN_POINT('Ctrl Pts',(-36.0340864334346,4.13905909688259,0.410798315377361));
#27529=CARTESIAN_POINT('Ctrl Pts',(-36.0479110832572,4.10691957881801,-0.668650461754651));
#27530=CARTESIAN_POINT('Ctrl Pts',(-36.054743369101,3.98241785588811,-1.20591830893745));
#27531=CARTESIAN_POINT('Ctrl Pts',(-36.0670127170578,3.54154333993596,-2.17832645881722));
#27532=CARTESIAN_POINT('Ctrl Pts',(-36.0729205373609,3.23803788616501,-2.60820919952761));
#27533=CARTESIAN_POINT('Ctrl Pts',(-36.0862432780018,2.47370737118609,-3.34484086675196));
#27534=CARTESIAN_POINT('Ctrl Pts',(-36.0932361557912,2.01509670145264,-3.63958423728565));
#27535=CARTESIAN_POINT('Ctrl Pts',(-36.1065821902674,1.03078125812558,-4.02759302272963));
#27536=CARTESIAN_POINT('Ctrl Pts',(-36.1126283245692,0.517550452608532,
-4.12499999586171));
#27537=CARTESIAN_POINT('Ctrl Pts',(-36.1184904636295,3.29830760293365E-8,
-4.12499999999999));
#27538=CARTESIAN_POINT('Origin',(-44.,0.,0.));
#27539=CARTESIAN_POINT('',(-44.,-5.08228421646152E-16,-4.15));
#27540=CARTESIAN_POINT('',(-44.,-5.08228421646152E-16,-4.15));
#27541=CARTESIAN_POINT('Origin',(-44.,0.,0.));
#27542=CARTESIAN_POINT('Origin',(0.,0.,0.));
#27543=CARTESIAN_POINT('',(-36.,-9.79717439317882E-16,8.));
#27544=CARTESIAN_POINT('Origin',(-36.,0.,0.));
#27545=CARTESIAN_POINT('',(-34.5,-9.79717439317882E-16,8.));
#27546=CARTESIAN_POINT('',(0.,-9.79717439317882E-16,8.));
#27547=CARTESIAN_POINT('',(-34.5,-2.47065947129021,7.60893171062298));
#27548=CARTESIAN_POINT('Origin',(-34.5,0.,0.));
#27549=CARTESIAN_POINT('',(-27.5,-2.47065947129021,7.60893171062298));
#27550=CARTESIAN_POINT('Ctrl Pts',(-27.5,-2.47065947129021,7.60893171062298));
#27551=CARTESIAN_POINT('Ctrl Pts',(-27.5082762748436,-2.53363768497578,
7.58848235898667));
#27552=CARTESIAN_POINT('Ctrl Pts',(-27.5167952547663,-2.59610030182682,
7.56728331237343));
#27553=CARTESIAN_POINT('Ctrl Pts',(-27.531909539296,-2.69176254620422,7.5336703249928));
#27554=CARTESIAN_POINT('Ctrl Pts',(-27.541703143922,-2.74920364206476,7.51311905977958));
#27555=CARTESIAN_POINT('Ctrl Pts',(-27.5886747936238,-2.94732068709103,
7.43861628862778));
#27556=CARTESIAN_POINT('Ctrl Pts',(-27.6278318406471,-3.044268769857,7.39878659172515));
#27557=CARTESIAN_POINT('Ctrl Pts',(-27.8123603858098,-3.37981144694253,
7.25589234200809));
#27558=CARTESIAN_POINT('Ctrl Pts',(-28.022658308916,-3.57168495780948,7.15984048137768));
#27559=CARTESIAN_POINT('Ctrl Pts',(-28.336993665887,-3.81265791239897,7.03423030810345));
#27560=CARTESIAN_POINT('Ctrl Pts',(-28.4851452188162,-3.89961660935025,
6.98559531051076));
#27561=CARTESIAN_POINT('Ctrl Pts',(-28.7988210742809,-4.06294287716043,
6.89241495700718));
#27562=CARTESIAN_POINT('Ctrl Pts',(-29.0017446327031,-4.14499080192856,
6.84289918755403));
#27563=CARTESIAN_POINT('Ctrl Pts',(-29.4670154464834,-4.29594038338126,
6.74941755583053));
#27564=CARTESIAN_POINT('Ctrl Pts',(-29.7360700177731,-4.35777776217867,
6.70912896172516));
#27565=CARTESIAN_POINT('Ctrl Pts',(-30.3331963799111,-4.45215289547283,
6.64696430829746));
#27566=CARTESIAN_POINT('Ctrl Pts',(-30.667122960172,-4.47714488295397,6.62986981008182));
#27567=CARTESIAN_POINT('Ctrl Pts',(-31.4223356644344,-4.47722023321691,
6.62981892557196));
#27568=CARTESIAN_POINT('Ctrl Pts',(-31.7581570009252,-4.43692246189483,
6.65701260246374));
#27569=CARTESIAN_POINT('Ctrl Pts',(-32.4245916936501,-4.33028864634714,
6.72720608258351));
#27570=CARTESIAN_POINT('Ctrl Pts',(-32.9726605932112,-4.20069539173016,
6.81615080651099));
#27571=CARTESIAN_POINT('Ctrl Pts',(-33.620923016355,-3.83675530423863,7.02052775006877));
#27572=CARTESIAN_POINT('Ctrl Pts',(-33.7554605943269,-3.74680811900599,
7.0692841494146));
#27573=CARTESIAN_POINT('Ctrl Pts',(-33.9780038810456,-3.56413110131904,
7.16275145624606));
#27574=CARTESIAN_POINT('Ctrl Pts',(-34.0686873290645,-3.47735595456888,
7.20546101456539));
#27575=CARTESIAN_POINT('Ctrl Pts',(-34.1772650516204,-3.35016875610881,
7.26482911701887));
#27576=CARTESIAN_POINT('Ctrl Pts',(-34.2047645004423,-3.31541359912121,
7.2807667169273));
#27577=CARTESIAN_POINT('Ctrl Pts',(-34.2531499977949,-3.24829608019548,
7.3109342508995));
#27578=CARTESIAN_POINT('Ctrl Pts',(-34.2735415360389,-3.21738266753306,
7.32459320987789));
#27579=CARTESIAN_POINT('Ctrl Pts',(-34.3258608593232,-3.13079515769325,
7.36217786629595));
#27580=CARTESIAN_POINT('Ctrl Pts',(-34.3543988312875,-3.07492684441128,
7.38572796575362));
#27581=CARTESIAN_POINT('Ctrl Pts',(-34.4549669946965,-2.82653092707015,
7.48680369569123));
#27582=CARTESIAN_POINT('Ctrl Pts',(-34.4789671836597,-2.62428232032289,
7.55904957717719));
#27583=CARTESIAN_POINT('Ctrl Pts',(-34.5,-2.47065947129021,7.60893171062298));
#27584=CARTESIAN_POINT('',(-27.5,-9.79717439317882E-16,8.));
#27585=CARTESIAN_POINT('Origin',(-27.5,0.,0.));
#27586=CARTESIAN_POINT('',(-20.,-9.79717439317882E-16,8.));
#27587=CARTESIAN_POINT('',(0.,-9.79717439317882E-16,8.));
#27588=CARTESIAN_POINT('Origin',(-20.,0.,0.));
#27589=CARTESIAN_POINT('',(-27.5,6.19655913866284,5.0599066039853));
#27590=CARTESIAN_POINT('Origin',(-27.5,0.,0.));
#27591=CARTESIAN_POINT('',(-34.5,6.19655913866284,5.0599066039853));
#27592=CARTESIAN_POINT('Ctrl Pts',(-34.5,6.19655913866284,5.0599066039853));
#27593=CARTESIAN_POINT('Ctrl Pts',(-34.4917237251617,6.23843937773582,5.00861842843821));
#27594=CARTESIAN_POINT('Ctrl Pts',(-34.4832047452396,6.27948024728051,4.95697905290007));
#27595=CARTESIAN_POINT('Ctrl Pts',(-34.4680904607238,6.34171420244266,4.87692886408564));
#27596=CARTESIAN_POINT('Ctrl Pts',(-34.4582968560933,6.37888375730234,4.82855264885907));
#27597=CARTESIAN_POINT('Ctrl Pts',(-34.4113252064685,6.50512326594944,4.65865676098275));
#27598=CARTESIAN_POINT('Ctrl Pts',(-34.3721681594988,6.56507277118939,4.57268355368093));
#27599=CARTESIAN_POINT('Ctrl Pts',(-34.1876396142192,6.76983200977991,4.27088675275452));
#27600=CARTESIAN_POINT('Ctrl Pts',(-33.9773416916577,6.87915596409205,4.08625285297235));
#27601=CARTESIAN_POINT('Ctrl Pts',(-33.6630063342077,7.01375978486032,3.85018571820814));
#27602=CARTESIAN_POINT('Ctrl Pts',(-33.5148547815411,7.06054343608664,3.76221715605519));
#27603=CARTESIAN_POINT('Ctrl Pts',(-33.2011789257173,7.14741992935041,3.59545228256026));
#27604=CARTESIAN_POINT('Ctrl Pts',(-32.9982553672152,7.1895978636344,3.5094017436486));
#27605=CARTESIAN_POINT('Ctrl Pts',(-32.5329845533841,7.2659051532144,3.34908396804489));
#27606=CARTESIAN_POINT('Ctrl Pts',(-32.2639299821026,7.29608576292504,3.28173292478837));
#27607=CARTESIAN_POINT('Ctrl Pts',(-31.6668036200137,7.34178042907256,3.1783738061678));
#27608=CARTESIAN_POINT('Ctrl Pts',(-31.332877039813,7.35353874703556,3.15047105961028));
#27609=CARTESIAN_POINT('Ctrl Pts',(-30.5776643347629,7.353574552694,3.15038748419466));
#27610=CARTESIAN_POINT('Ctrl Pts',(-30.2418429982892,7.33441482688859,3.1950675844706));
#27611=CARTESIAN_POINT('Ctrl Pts',(-29.5754083083462,7.28275986922452,3.31181372141937));
#27612=CARTESIAN_POINT('Ctrl Pts',(-29.02733940778,7.22195244224698,3.45675520013408));
#27613=CARTESIAN_POINT('Ctrl Pts',(-28.3790769835261,7.02660224834134,3.82561916527211));
#27614=CARTESIAN_POINT('Ctrl Pts',(-28.2445394054004,6.97737165243015,3.91530768774012));
#27615=CARTESIAN_POINT('Ctrl Pts',(-28.0219961187517,6.87438073889736,4.09278980501267));
#27616=CARTESIAN_POINT('Ctrl Pts',(-27.9313126708239,6.82454353901441,4.17567699316933));
#27617=CARTESIAN_POINT('Ctrl Pts',(-27.8227349483168,6.74974708920182,4.29444839597648));
#27618=CARTESIAN_POINT('Ctrl Pts',(-27.7952354994949,6.72915375666957,4.32666396183648));
#27619=CARTESIAN_POINT('Ctrl Pts',(-27.7468500021218,6.68905442683588,4.3883639229692));
#27620=CARTESIAN_POINT('Ctrl Pts',(-27.7264584638972,6.67045756991583,4.41658383000757));
#27621=CARTESIAN_POINT('Ctrl Pts',(-27.6741391406086,6.61800364689995,4.49506050949652));
#27622=CARTESIAN_POINT('Ctrl Pts',(-27.6456011686512,6.58377994863887,4.54510662916641));
#27623=CARTESIAN_POINT('Ctrl Pts',(-27.5450330043088,6.4296527386651,4.76456423198599));
#27624=CARTESIAN_POINT('Ctrl Pts',(-27.5210328155748,6.29871766361913,4.93479928660682));
#27625=CARTESIAN_POINT('Ctrl Pts',(-27.5,6.19655913866284,5.0599066039853));
#27626=CARTESIAN_POINT('Origin',(-34.5,0.,0.));
#27627=CARTESIAN_POINT('Origin',(-43.,0.,0.));
#27628=CARTESIAN_POINT('',(-43.,-1.53080849893419E-15,12.5));
#27629=CARTESIAN_POINT('Origin',(-43.,0.,0.));
#27630=CARTESIAN_POINT('',(-44.,-1.40834381901945E-15,11.5));
#27631=CARTESIAN_POINT('Origin',(-43.,-1.40834381901945E-15,11.5));
#27632=CARTESIAN_POINT('Origin',(-44.,0.,0.));
#27633=CARTESIAN_POINT('Origin',(0.,0.,0.));
#27634=CARTESIAN_POINT('',(-25.,-1.53080849893419E-15,12.5));
#27635=CARTESIAN_POINT('Origin',(-25.,0.,0.));
#27636=CARTESIAN_POINT('',(-27.5,-1.53080849893419E-15,12.5));
#27637=CARTESIAN_POINT('',(0.,-1.53080849893419E-15,12.5));
#27638=CARTESIAN_POINT('',(-27.5,-3.86040542389096,11.8889557978484));
#27639=CARTESIAN_POINT('Origin',(-27.5,0.,0.));
#27640=CARTESIAN_POINT('',(-34.5,-3.86040542389096,11.8889557978484));
#27641=CARTESIAN_POINT('Ctrl Pts',(-34.5,-3.86040542389096,11.8889557978484));
#27642=CARTESIAN_POINT('Ctrl Pts',(-34.494970655399,-3.91780250120729,11.8703186700506));
#27643=CARTESIAN_POINT('Ctrl Pts',(-34.4903159600402,-3.96935886536347,
11.8531231208353));
#27644=CARTESIAN_POINT('Ctrl Pts',(-34.4860358608515,-4.01514468999518,
11.8375932147715));
#27645=CARTESIAN_POINT('Ctrl Pts',(-34.4848922703583,-4.02737810596607,
11.8334438125843));
#27646=CARTESIAN_POINT('Ctrl Pts',(-34.4837754220408,-4.03919950769951,
11.8294130376282));
#27647=CARTESIAN_POINT('Ctrl Pts',(-34.4826853148868,-4.05061009613366,
11.8255045494516));
#27648=CARTESIAN_POINT('Ctrl Pts',(-34.4801002973656,-4.07766851045364,
11.8162361849796));
#27649=CARTESIAN_POINT('Ctrl Pts',(-34.4776656615101,-4.10241686090276,
11.8076560597129));
#27650=CARTESIAN_POINT('Ctrl Pts',(-34.4753814073201,-4.1248695117463,11.799807265844));
#27651=CARTESIAN_POINT('Ctrl Pts',(-34.4742392802251,-4.13609583716807,
11.7958828689096));
#27652=CARTESIAN_POINT('Ctrl Pts',(-34.4731347485465,-4.14674820379434,
11.7921411785115));
#27653=CARTESIAN_POINT('Ctrl Pts',(-34.4720678122842,-4.15682819390705,
11.7885868265174));
#27654=CARTESIAN_POINT('Ctrl Pts',(-34.4713134278961,-4.1639553180311,11.7860736982743));
#27655=CARTESIAN_POINT('Ctrl Pts',(-34.47090989401,-4.16780274964417,11.784713577999));
#27656=CARTESIAN_POINT('Ctrl Pts',(-34.4701528645571,-4.17472128216715,
11.7822621858547));
#27657=CARTESIAN_POINT('Ctrl Pts',(-34.4698392167961,-4.17758772577372,
11.7812465402223));
#27658=CARTESIAN_POINT('Ctrl Pts',(-34.4694648894221,-4.1809812090102,11.7800431939136));
#27659=CARTESIAN_POINT('Ctrl Pts',(-34.4689797897467,-4.18535246715401,
11.7784899170347));
#27660=CARTESIAN_POINT('Ctrl Pts',(-34.4623559877182,-4.24503988817323,
11.7572806706389));
#27661=CARTESIAN_POINT('Ctrl Pts',(-34.4552691208995,-4.3014092606901,11.73674089348));
#27662=CARTESIAN_POINT('Ctrl Pts',(-34.4477191892904,-4.35450417596821,
11.7170087215755));
#27663=CARTESIAN_POINT('Ctrl Pts',(-34.4439442234859,-4.38105163360727,
11.7071426356232));
#27664=CARTESIAN_POINT('Ctrl Pts',(-34.4400534914838,-4.40678045394109,
11.6974781922229));
#27665=CARTESIAN_POINT('Ctrl Pts',(-34.4360469932842,-4.43169590229857,
11.688031118608));
#27666=CARTESIAN_POINT('Ctrl Pts',(-34.4336061624609,-4.44687484193522,
11.6822757913073));
#27667=CARTESIAN_POINT('Ctrl Pts',(-34.4314324547114,-4.46004496983625,
11.6772527958857));
#27668=CARTESIAN_POINT('Ctrl Pts',(-34.4289591340832,-4.4743282340168,11.6717773648352));
#27669=CARTESIAN_POINT('Ctrl Pts',(-34.4273726261688,-4.48349021302091,
11.6682651575633));
#27670=CARTESIAN_POINT('Ctrl Pts',(-34.4256628406678,-4.49310990046616,
11.6645659967412));
#27671=CARTESIAN_POINT('Ctrl Pts',(-34.4236802000926,-4.50400723835645,
11.6603567182498));
#27672=CARTESIAN_POINT('Ctrl Pts',(-34.4154020416518,-4.54950710896653,
11.6427816344403));
#27673=CARTESIAN_POINT('Ctrl Pts',(-34.406653472996,-4.59275567416098,11.6257749226861));
#27674=CARTESIAN_POINT('Ctrl Pts',(-34.3971295455735,-4.63477689237434,
11.60899837014));
#27675=CARTESIAN_POINT('Ctrl Pts',(-34.3873134488299,-4.67808721226327,
11.5917071565984));
#27676=CARTESIAN_POINT('Ctrl Pts',(-34.3766736916467,-4.72009374737927,
11.5746602240549));
#27677=CARTESIAN_POINT('Ctrl Pts',(-34.3648763906193,-4.76189818145385,
11.5574359487503));
#27678=CARTESIAN_POINT('Ctrl Pts',(-34.3600593412814,-4.77896768074119,
11.5504029686001));
#27679=CARTESIAN_POINT('Ctrl Pts',(-34.3550493021611,-4.79600326253241,
11.5433398564416));
#27680=CARTESIAN_POINT('Ctrl Pts',(-34.3498235437455,-4.81307899502436,
11.5362156094473));
#27681=CARTESIAN_POINT('Ctrl Pts',(-34.3365616064945,-4.85641381359207,
11.5181356851409));
#27682=CARTESIAN_POINT('Ctrl Pts',(-34.3215920418828,-4.90045195053886,
11.49947096044));
#27683=CARTESIAN_POINT('Ctrl Pts',(-34.3053895006549,-4.94413101835602,
11.4806606287848));
#27684=CARTESIAN_POINT('Ctrl Pts',(-34.2889938068611,-4.98833078992604,
11.4616260567607));
#27685=CARTESIAN_POINT('Ctrl Pts',(-34.2713355642849,-5.03216278653615,
11.4424424259165));
#27686=CARTESIAN_POINT('Ctrl Pts',(-34.2529066019543,-5.07454774569108,
11.4236143657208));
#27687=CARTESIAN_POINT('Ctrl Pts',(-34.2477440704824,-5.0864211046815,11.4183400343953));
#27688=CARTESIAN_POINT('Ctrl Pts',(-34.2425210578452,-5.0981810411742,11.4130938957045));
#27689=CARTESIAN_POINT('Ctrl Pts',(-34.2372483758835,-5.10980413280796,
11.407887697744));
#27690=CARTESIAN_POINT('Ctrl Pts',(-34.2060970380929,-5.17847409171857,
11.3771291516276));
#27691=CARTESIAN_POINT('Ctrl Pts',(-34.1713309554745,-5.24692483123779,
11.3457195635697));
#27692=CARTESIAN_POINT('Ctrl Pts',(-34.1334397960299,-5.31449179121027,
11.3139814831543));
#27693=CARTESIAN_POINT('Ctrl Pts',(-34.0948626907383,-5.38328191975986,
11.2816688464369));
#27694=CARTESIAN_POINT('Ctrl Pts',(-34.0530463375756,-5.45115583394936,
11.2490157906367));
#27695=CARTESIAN_POINT('Ctrl Pts',(-34.0085074823357,-5.51743673946892,
11.2164117179229));
#27696=CARTESIAN_POINT('Ctrl Pts',(-33.9768762953056,-5.56450898027351,
11.1932565309205));
#27697=CARTESIAN_POINT('Ctrl Pts',(-33.9438719484171,-5.61077827891772,
11.1701271129436));
#27698=CARTESIAN_POINT('Ctrl Pts',(-33.9096795416066,-5.65600990849816,
11.1471768585131));
#27699=CARTESIAN_POINT('Ctrl Pts',(-33.8448661510052,-5.74174868938547,
11.1036735212649));
#27700=CARTESIAN_POINT('Ctrl Pts',(-33.7764476368752,-5.82327304054431,
11.0610704051755));
#27701=CARTESIAN_POINT('Ctrl Pts',(-33.7039936885002,-5.90106683527327,
11.0194106106288));
#27702=CARTESIAN_POINT('Ctrl Pts',(-33.6315397401253,-5.97886063000223,
10.977750816082));
#27703=CARTESIAN_POINT('Ctrl Pts',(-33.5550503575055,-6.05292387508725,
10.9370337816686));
#27704=CARTESIAN_POINT('Ctrl Pts',(-33.4740952299247,-6.12372280736542,
10.8972482296474));
#27705=CARTESIAN_POINT('Ctrl Pts',(-33.3673080229709,-6.21711306514419,
10.8447674528959));
#27706=CARTESIAN_POINT('Ctrl Pts',(-33.2534811611839,-6.30331921585543,
10.7947479660883));
#27707=CARTESIAN_POINT('Ctrl Pts',(-33.1337150622316,-6.38220287634025,
10.7479061423718));
#27708=CARTESIAN_POINT('Ctrl Pts',(-33.0200172364479,-6.45708968291937,
10.703437686282));
#27709=CARTESIAN_POINT('Ctrl Pts',(-32.9009667812065,-6.52537806498607,
10.6618332745438));
#27710=CARTESIAN_POINT('Ctrl Pts',(-32.777505179161,-6.58694495509603,10.6236602053405));
#27711=CARTESIAN_POINT('Ctrl Pts',(-32.6598228499643,-6.64562988149819,
10.5872740284077));
#27712=CARTESIAN_POINT('Ctrl Pts',(-32.5381326823293,-6.69820844752292,
10.5540056089092));
#27713=CARTESIAN_POINT('Ctrl Pts',(-32.4132500380636,-6.74455973963733,
10.5243011130651));
#27714=CARTESIAN_POINT('Ctrl Pts',(-32.2959024600774,-6.78811432560992,
10.4963889026607));
#27715=CARTESIAN_POINT('Ctrl Pts',(-32.1757360330685,-6.82617076458576,
10.4716234758828));
#27716=CARTESIAN_POINT('Ctrl Pts',(-32.0534272550074,-6.85860954795537,
10.4503337300153));
#27717=CARTESIAN_POINT('Ctrl Pts',(-31.934697526644,-6.89009909432292,10.4296669734354));
#27718=CARTESIAN_POINT('Ctrl Pts',(-31.8139489934702,-6.91629525531148,
10.4122756081045));
#27719=CARTESIAN_POINT('Ctrl Pts',(-31.691800486454,-6.93706541972051,10.3984192722989));
#27720=CARTESIAN_POINT('Ctrl Pts',(-31.5747340084618,-6.95697143457143,
10.3851394339263));
#27721=CARTESIAN_POINT('Ctrl Pts',(-31.4563816260168,-6.97189371437512,
10.3751066275311));
#27722=CARTESIAN_POINT('Ctrl Pts',(-31.3372880991137,-6.98169062285308,
10.3685098276833));
#27723=CARTESIAN_POINT('Ctrl Pts',(-31.2253150028751,-6.99090178826543,
10.3623074410093));
#27724=CARTESIAN_POINT('Ctrl Pts',(-31.1126867367521,-6.9955821236098,10.3591423753097));
#27725=CARTESIAN_POINT('Ctrl Pts',(-30.9998560750767,-6.99559063859199,
10.3591366250882));
#27726=CARTESIAN_POINT('Ctrl Pts',(-30.8797994738452,-6.99559969889357,
10.3591305066091));
#27727=CARTESIAN_POINT('Ctrl Pts',(-30.7600926671373,-6.99048466724076,
10.3625901353736));
#27728=CARTESIAN_POINT('Ctrl Pts',(-30.6411870533517,-6.98031808007771,
10.3694339045553));
#27729=CARTESIAN_POINT('Ctrl Pts',(-30.5209337732766,-6.97003626566538,
10.3763552404449));
#27730=CARTESIAN_POINT('Ctrl Pts',(-30.4014999503503,-6.95458763079492,
10.3867377989898));
#27731=CARTESIAN_POINT('Ctrl Pts',(-30.2833525059205,-6.93401732448088,
10.4004520932409));
#27732=CARTESIAN_POINT('Ctrl Pts',(-30.1629637338705,-6.91305678716422,
10.414426555849));
#27733=CARTESIAN_POINT('Ctrl Pts',(-30.043910610001,-6.88677828371061,10.4318603772502));
#27734=CARTESIAN_POINT('Ctrl Pts',(-29.9266871362902,-6.85520048168457,
10.4525703229355));
#27735=CARTESIAN_POINT('Ctrl Pts',(-29.8368473729342,-6.8309993368838,10.4684423710892));
#27736=CARTESIAN_POINT('Ctrl Pts',(-29.7480822819468,-6.80368493907954,
10.4862377470792));
#27737=CARTESIAN_POINT('Ctrl Pts',(-29.6606142407677,-6.77325535385644,
10.5058560770389));
#27738=CARTESIAN_POINT('Ctrl Pts',(-29.5206149476823,-6.72455047419196,
10.5372567153617));
#27739=CARTESIAN_POINT('Ctrl Pts',(-29.3844295684138,-6.66785803981784,
10.57333373119));
#27740=CARTESIAN_POINT('Ctrl Pts',(-29.2532397481725,-6.60365955267175,
10.61327849971));
#27741=CARTESIAN_POINT('Ctrl Pts',(-29.1018107116331,-6.52955688953876,
10.6593857190099));
#27742=CARTESIAN_POINT('Ctrl Pts',(-28.9570375038436,-6.44545120919904,
10.710644896099));
#27743=CARTESIAN_POINT('Ctrl Pts',(-28.8207373726615,-6.35207155220489,
10.7657413583863));
#27744=CARTESIAN_POINT('Ctrl Pts',(-28.7172009582184,-6.28113842262358,
10.8075937770468));
#27745=CARTESIAN_POINT('Ctrl Pts',(-28.6185537102732,-6.2048534694645,10.8516584751742));
#27746=CARTESIAN_POINT('Ctrl Pts',(-28.525592163538,-6.1235467477601,10.8973471647001));
#27747=CARTESIAN_POINT('Ctrl Pts',(-28.4641697382623,-6.06982500781815,
10.9275350242712));
#27748=CARTESIAN_POINT('Ctrl Pts',(-28.4054615364755,-6.01445977844525,
10.9581285073625));
#27749=CARTESIAN_POINT('Ctrl Pts',(-28.3489685850519,-5.95676427999888,
10.9894021362643));
#27750=CARTESIAN_POINT('Ctrl Pts',(-28.2950240546477,-5.9016714499785,11.019264998491));
#27751=CARTESIAN_POINT('Ctrl Pts',(-28.2430994207628,-5.84445379489708,
11.0497481752732));
#27752=CARTESIAN_POINT('Ctrl Pts',(-28.192760236588,-5.78449380851062,11.0810482978508));
#27753=CARTESIAN_POINT('Ctrl Pts',(-28.1579080059993,-5.74298063530583,
11.1027188733162));
#27754=CARTESIAN_POINT('Ctrl Pts',(-28.1238157538695,-5.70015254261527,
11.1247802072868));
#27755=CARTESIAN_POINT('Ctrl Pts',(-28.0903392986022,-5.65579883898769,
11.1472839513895));
#27756=CARTESIAN_POINT('Ctrl Pts',(-28.0241068899402,-5.56804604076333,
11.1918070994926));
#27757=CARTESIAN_POINT('Ctrl Pts',(-27.9636909773592,-5.47865680552519,
11.2358577237503));
#27758=CARTESIAN_POINT('Ctrl Pts',(-27.9090915608592,-5.38761723205833,
11.2793430908377));
#27759=CARTESIAN_POINT('Ctrl Pts',(-27.8843690560396,-5.34639469822763,
11.2990331766722));
#27760=CARTESIAN_POINT('Ctrl Pts',(-27.8612040828302,-5.30562818737182,
11.318232711205));
#27761=CARTESIAN_POINT('Ctrl Pts',(-27.8391008292385,-5.26424125835,11.3374496238742));
#27762=CARTESIAN_POINT('Ctrl Pts',(-27.8174064239111,-5.22361987156048,
11.3563110774994));
#27763=CARTESIAN_POINT('Ctrl Pts',(-27.7967348237883,-5.18240074233437,
11.3751893510415));
#27764=CARTESIAN_POINT('Ctrl Pts',(-27.7766172244931,-5.1395454600324,11.3945194047077));
#27765=CARTESIAN_POINT('Ctrl Pts',(-27.77196471905,-5.12963451433504,11.3989897780648));
#27766=CARTESIAN_POINT('Ctrl Pts',(-27.7673418436229,-5.11963597385404,
11.4034841144338));
#27767=CARTESIAN_POINT('Ctrl Pts',(-27.7627427996022,-5.10953683452028,
11.4080074218367));
#27768=CARTESIAN_POINT('Ctrl Pts',(-27.7433129351307,-5.06687037869769,
11.4271173171552));
#27769=CARTESIAN_POINT('Ctrl Pts',(-27.7249399287126,-5.0232704538905,11.4463531880018));
#27770=CARTESIAN_POINT('Ctrl Pts',(-27.7079530152698,-4.97978848766015,
11.4652390563026));
#27771=CARTESIAN_POINT('Ctrl Pts',(-27.6907728782746,-4.93581192068873,
11.484339748478));
#27772=CARTESIAN_POINT('Ctrl Pts',(-27.6750105467902,-4.89195610261451,
11.5030823858444));
#27773=CARTESIAN_POINT('Ctrl Pts',(-27.6610066190104,-4.84933007757205,
11.5210241644897));
#27774=CARTESIAN_POINT('Ctrl Pts',(-27.6569688649967,-4.83703971115383,
11.5261973194701));
#27775=CARTESIAN_POINT('Ctrl Pts',(-27.6530772945585,-4.82485171033533,
11.5313042061676));
#27776=CARTESIAN_POINT('Ctrl Pts',(-27.6493400718713,-4.81279295543508,
11.5363349452118));
#27777=CARTESIAN_POINT('Ctrl Pts',(-27.6345827386579,-4.76517602727854,
11.5562000425308));
#27778=CARTESIAN_POINT('Ctrl Pts',(-27.6209916578288,-4.715632537521,11.5765232413219));
#27779=CARTESIAN_POINT('Ctrl Pts',(-27.6085668293839,-4.664138015756,11.5972331428656));
#27780=CARTESIAN_POINT('Ctrl Pts',(-27.6023544151614,-4.63839075487349,
11.6075880936374));
#27781=CARTESIAN_POINT('Ctrl Pts',(-27.596433564035,-4.61215573118547,11.6180396300778));
#27782=CARTESIAN_POINT('Ctrl Pts',(-27.5908042760046,-4.5854298718991,11.6285782832595));
#27783=CARTESIAN_POINT('Ctrl Pts',(-27.5873939612376,-4.56923890918867,
11.6349627717377));
#27784=CARTESIAN_POINT('Ctrl Pts',(-27.5837940741683,-4.5512419425587,11.642015449446));
#27785=CARTESIAN_POINT('Ctrl Pts',(-27.5805436336287,-4.53439193817792,
11.6485745802217));
#27786=CARTESIAN_POINT('Ctrl Pts',(-27.5784286849673,-4.52342822609788,
11.652842378597));
#27787=CARTESIAN_POINT('Ctrl Pts',(-27.5764616798231,-4.51295056810901,
11.6569024137903));
#27788=CARTESIAN_POINT('Ctrl Pts',(-27.5747911012017,-4.50377671744548,
11.6604457581773));
#27789=CARTESIAN_POINT('Ctrl Pts',(-27.566314957399,-4.45723064265866,11.6784238983155));
#27790=CARTESIAN_POINT('Ctrl Pts',(-27.5583409045667,-4.40744011781925,
11.6973363546891));
#27791=CARTESIAN_POINT('Ctrl Pts',(-27.5508689427049,-4.3543635178157,11.717060994751));
#27792=CARTESIAN_POINT('Ctrl Pts',(-27.5471329617739,-4.32782521781393,
11.726923314782));
#27793=CARTESIAN_POINT('Ctrl Pts',(-27.5435225035856,-4.300465355621,11.7369884258351));
#27794=CARTESIAN_POINT('Ctrl Pts',(-27.5400375681399,-4.27227851169748,
11.7472395190737));
#27795=CARTESIAN_POINT('Ctrl Pts',(-27.538295100417,-4.25818508973572,11.7523650656931));
#27796=CARTESIAN_POINT('Ctrl Pts',(-27.5365840133798,-4.24388492044556,
11.7575370916891));
#27797=CARTESIAN_POINT('Ctrl Pts',(-27.5349043070283,-4.22937731649073,
11.7627533985353));
#27798=CARTESIAN_POINT('Ctrl Pts',(-27.533779193636,-4.21965972538717,11.7662474239554));
#27799=CARTESIAN_POINT('Ctrl Pts',(-27.5323768483603,-4.20716236796442,
11.7707219324888));
#27800=CARTESIAN_POINT('Ctrl Pts',(-27.5312826563378,-4.19728311588018,
11.7742436888807));
#27801=CARTESIAN_POINT('Ctrl Pts',(-27.5307433051967,-4.19241341680146,
11.7759796395084));
#27802=CARTESIAN_POINT('Ctrl Pts',(-27.5302788266484,-4.18818021743347,
11.7774851415309));
#27803=CARTESIAN_POINT('Ctrl Pts',(-27.5299593300305,-4.1852315079248,11.7785328978219));
#27804=CARTESIAN_POINT('Ctrl Pts',(-27.5269020793694,-4.15701542177606,
11.788558836859));
#27805=CARTESIAN_POINT('Ctrl Pts',(-27.5234947220653,-4.12310099413958,
11.8004999619284));
#27806=CARTESIAN_POINT('Ctrl Pts',(-27.5197371907049,-4.08343722589056,
11.8142092592865));
#27807=CARTESIAN_POINT('Ctrl Pts',(-27.5159831432012,-4.04381023255444,
11.8279058458449));
#27808=CARTESIAN_POINT('Ctrl Pts',(-27.5118795706794,-3.99844438731281,
11.8433673740677));
#27809=CARTESIAN_POINT('Ctrl Pts',(-27.5074264059136,-3.94727538011812,
11.8603970031999));
#27810=CARTESIAN_POINT('Ctrl Pts',(-27.5050504578766,-3.91997459324096,
11.8694830164142));
#27811=CARTESIAN_POINT('Ctrl Pts',(-27.5025749926422,-3.89102162637507,
11.8790145585892));
#27812=CARTESIAN_POINT('Ctrl Pts',(-27.5,-3.86040542389096,11.8889557978484));
#27813=CARTESIAN_POINT('',(-34.5,-1.53080849893419E-15,12.5));
#27814=CARTESIAN_POINT('Origin',(-34.5,0.,0.));
#27815=CARTESIAN_POINT('',(0.,-1.53080849893419E-15,12.5));
#27816=CARTESIAN_POINT('',(-34.5,9.68212365416069,7.90610406872703));
#27817=CARTESIAN_POINT('Origin',(-34.5,0.,0.));
#27818=CARTESIAN_POINT('',(-27.5,9.68212365416069,7.90610406872703));
#27819=CARTESIAN_POINT('Ctrl Pts',(-27.5,9.68212365416069,7.90610406872703));
#27820=CARTESIAN_POINT('Ctrl Pts',(-27.5050293446173,9.72029246189198,7.85936105687521));
#27821=CARTESIAN_POINT('Ctrl Pts',(-27.509684039994,9.75433093310758,7.8169921048418));
#27822=CARTESIAN_POINT('Ctrl Pts',(-27.5139641392024,9.78441937113138,7.77914761203495));
#27823=CARTESIAN_POINT('Ctrl Pts',(-27.5151077296653,9.79245863589893,7.76903602374222));
#27824=CARTESIAN_POINT('Ctrl Pts',(-27.5162245779542,9.80021570799085,7.75924722860733));
#27825=CARTESIAN_POINT('Ctrl Pts',(-27.5173146850816,9.80769357831618,7.74978365335804));
#27826=CARTESIAN_POINT('Ctrl Pts',(-27.5198997026027,9.82542617112911,7.72734227377413));
#27827=CARTESIAN_POINT('Ctrl Pts',(-27.5223343384609,9.84158909730558,7.70673016037892));
#27828=CARTESIAN_POINT('Ctrl Pts',(-27.5246185926562,9.85621776302709,7.68797576789816));
#27829=CARTESIAN_POINT('Ctrl Pts',(-27.5257607197538,9.86353209588784,7.67859857165778));
#27830=CARTESIAN_POINT('Ctrl Pts',(-27.5268652514357,9.87046276675478,7.66968571779361));
#27831=CARTESIAN_POINT('Ctrl Pts',(-27.5279321877019,9.8770136135519,7.66124024409301));
#27832=CARTESIAN_POINT('Ctrl Pts',(-27.5286865720957,9.88164543341441,7.65526881565846));
#27833=CARTESIAN_POINT('Ctrl Pts',(-27.5290901059915,9.88414395336477,7.65204235381507));
#27834=CARTESIAN_POINT('Ctrl Pts',(-27.5298471354527,9.88863381537631,7.6462357579005));
#27835=CARTESIAN_POINT('Ctrl Pts',(-27.5301607832131,9.89049402721282,7.64383000502382));
#27836=CARTESIAN_POINT('Ctrl Pts',(-27.5305351105845,9.89269574853726,7.64098111157456));
#27837=CARTESIAN_POINT('Ctrl Pts',(-27.5310202102533,9.89553012268088,7.63730866150605));
#27838=CARTESIAN_POINT('Ctrl Pts',(-27.5398433802358,9.94708275500642,7.57051279810824));
#27839=CARTESIAN_POINT('Ctrl Pts',(-27.5494881803974,9.99432970581515,7.50790437538638));
#27840=CARTESIAN_POINT('Ctrl Pts',(-27.5599546107381,10.0375302558491,7.44969706517753));
#27841=CARTESIAN_POINT('Ctrl Pts',(-27.5612743460859,10.0429775087394,7.44235757670973));
#27842=CARTESIAN_POINT('Ctrl Pts',(-27.5626071447339,10.0483603838342,7.4350880100706));
#27843=CARTESIAN_POINT('Ctrl Pts',(-27.5639530066821,10.0536793631385,7.42788874870938));
#27844=CARTESIAN_POINT('Ctrl Pts',(-27.5663938375238,10.063325767623,7.41483229875763));
#27845=CARTESIAN_POINT('Ctrl Pts',(-27.568567545298,10.0716796635466,7.40347909748433));
#27846=CARTESIAN_POINT('Ctrl Pts',(-27.5710408659523,10.0807245282707,7.39114287408391));
#27847=CARTESIAN_POINT('Ctrl Pts',(-27.5726273738604,10.0865263434891,7.38322982166737));
#27848=CARTESIAN_POINT('Ctrl Pts',(-27.5743371593522,10.0926117802312,7.37491179089848));
#27849=CARTESIAN_POINT('Ctrl Pts',(-27.5763197999075,10.0994952788321,7.36547317643938));
#27850=CARTESIAN_POINT('Ctrl Pts',(-27.584597958343,10.1282360870729,7.32606394227561));
#27851=CARTESIAN_POINT('Ctrl Pts',(-27.5933465269982,10.1553917388671,7.28835138187274));
#27852=CARTESIAN_POINT('Ctrl Pts',(-27.6028704544253,10.1816400610147,7.25149678810799));
#27853=CARTESIAN_POINT('Ctrl Pts',(-27.6126865511699,10.2086936134022,7.21351159128179));
#27854=CARTESIAN_POINT('Ctrl Pts',(-27.6233263083588,10.2347832137565,7.17643761582166));
#27855=CARTESIAN_POINT('Ctrl Pts',(-27.6351236093967,10.2606068824975,7.13932394578398));
#27856=CARTESIAN_POINT('Ctrl Pts',(-27.6399406587293,10.2711511490102,7.12416976951004));
#27857=CARTESIAN_POINT('Ctrl Pts',(-27.6449506978443,10.2816505856281,7.10900862079852));
#27858=CARTESIAN_POINT('Ctrl Pts',(-27.6501764562545,10.2921506834825,7.09377433447739));
#27859=CARTESIAN_POINT('Ctrl Pts',(-27.6634383936158,10.318797847224,7.05511274029871));
#27860=CARTESIAN_POINT('Ctrl Pts',(-27.6784079583481,10.3457197533343,7.01557869851392));
#27861=CARTESIAN_POINT('Ctrl Pts',(-27.6946104997106,10.3722609327256,6.97611662341272));
#27862=CARTESIAN_POINT('Ctrl Pts',(-27.7110061936436,10.3991185129152,6.93618411586059));
#27863=CARTESIAN_POINT('Ctrl Pts',(-27.7286644363738,10.4255861779289,6.89632538582838));
#27864=CARTESIAN_POINT('Ctrl Pts',(-27.7470933988766,10.4510296958037,6.85754900073121));
#27865=CARTESIAN_POINT('Ctrl Pts',(-27.7522559300769,10.4581572242717,6.84668651740537));
#27866=CARTESIAN_POINT('Ctrl Pts',(-27.7574789424365,10.4652046518517,6.83590914184789));
#27867=CARTESIAN_POINT('Ctrl Pts',(-27.7627516241165,10.4721586455432,6.82523943188631));
#27868=CARTESIAN_POINT('Ctrl Pts',(-27.7939029620164,10.5132432814802,6.76220210847511));
#27869=CARTESIAN_POINT('Ctrl Pts',(-27.8286690447497,10.5537911448996,6.69873608001519));
#27870=CARTESIAN_POINT('Ctrl Pts',(-27.8665602043162,10.593418105067,6.63547231561086));
#27871=CARTESIAN_POINT('Ctrl Pts',(-27.9051373097431,10.6337624343938,6.57106328360848));
#27872=CARTESIAN_POINT('Ctrl Pts',(-27.94695366305,10.6731521330382,6.50686404722303));
#27873=CARTESIAN_POINT('Ctrl Pts',(-27.9914925184439,10.7112289762066,6.44356840727803));
#27874=CARTESIAN_POINT('Ctrl Pts',(-28.0231237052372,10.7382708866487,6.39861628193517));
#27875=CARTESIAN_POINT('Ctrl Pts',(-28.0561280518637,10.7646516481519,6.35412051415379));
#27876=CARTESIAN_POINT('Ctrl Pts',(-28.0903204583934,10.7902569501729,6.31033715020414));
#27877=CARTESIAN_POINT('Ctrl Pts',(-28.1551338489782,10.8387930612383,6.22734362746644));
#27878=CARTESIAN_POINT('Ctrl Pts',(-28.2235523631422,10.8842731098111,6.14738857434825));
#27879=CARTESIAN_POINT('Ctrl Pts',(-28.2960063115382,10.9271272613901,6.07024627287762));
#27880=CARTESIAN_POINT('Ctrl Pts',(-28.3684602599343,10.9699814129692,5.993103971407));
#27881=CARTESIAN_POINT('Ctrl Pts',(-28.4449496425624,11.0102093693281,5.91877394588719));
#27882=CARTESIAN_POINT('Ctrl Pts',(-28.5259047700753,11.0481970286813,5.8469943060891));
#27883=CARTESIAN_POINT('Ctrl Pts',(-28.6326919773777,11.0983062210067,5.75231040513453));
#27884=CARTESIAN_POINT('Ctrl Pts',(-28.7465188395995,11.1437076193583,5.66358519690919));
#27885=CARTESIAN_POINT('Ctrl Pts',(-28.8662849390525,11.1846726988873,5.58149591227711));
#27886=CARTESIAN_POINT('Ctrl Pts',(-28.9799827651499,11.2235621718653,5.50356590327462));
#27887=CARTESIAN_POINT('Ctrl Pts',(-29.0990332207493,11.258454322916,5.43161614291703));
#27888=CARTESIAN_POINT('Ctrl Pts',(-29.2224948231837,11.2895527991727,5.36619023094518));
#27889=CARTESIAN_POINT('Ctrl Pts',(-29.3401771526212,11.3191955468423,5.30382692466527));
#27890=CARTESIAN_POINT('Ctrl Pts',(-29.4618673205163,11.3453920449199,5.24739079413951));
#27891=CARTESIAN_POINT('Ctrl Pts',(-29.5867499650525,11.3682821739022,5.19732242741757));
#27892=CARTESIAN_POINT('Ctrl Pts',(-29.7040975431676,11.3897911770851,5.15027504467817));
#27893=CARTESIAN_POINT('Ctrl Pts',(-29.8242639703085,11.4083810197703,5.10884997192939));
#27894=CARTESIAN_POINT('Ctrl Pts',(-29.9465727484996,11.4241292774221,5.07338843897716));
#27895=CARTESIAN_POINT('Ctrl Pts',(-30.0653024769371,11.4394167030838,5.03896459598184));
#27896=CARTESIAN_POINT('Ctrl Pts',(-30.1860510101812,11.4520267529344,5.01016034153001));
#27897=CARTESIAN_POINT('Ctrl Pts',(-30.3081995172601,11.4619884910358,4.9872657670674));
#27898=CARTESIAN_POINT('Ctrl Pts',(-30.4252659952594,11.4715357677252,4.96532372895557));
#27899=CARTESIAN_POINT('Ctrl Pts',(-30.5436183777033,11.4786506641909,4.9488097989972));
#27900=CARTESIAN_POINT('Ctrl Pts',(-30.6627119045943,11.4833164009267,4.93795954177513));
#27901=CARTESIAN_POINT('Ctrl Pts',(-30.7746849996166,11.4877031799272,4.9277580059347));
#27902=CARTESIAN_POINT('Ctrl Pts',(-30.8873132644994,11.4899248413375,4.92256306618016));
#27903=CARTESIAN_POINT('Ctrl Pts',(-31.0001439249233,11.4899288875684,4.9225536217112));
#27904=CARTESIAN_POINT('Ctrl Pts',(-31.1202005261559,11.4899331929294,4.92254357239623));
#27905=CARTESIAN_POINT('Ctrl Pts',(-31.2399073328591,11.4875055150522,4.92822150864965));
#27906=CARTESIAN_POINT('Ctrl Pts',(-31.3588129466378,11.4826626615451,4.93947954759988));
#27907=CARTESIAN_POINT('Ctrl Pts',(-31.4790662266949,11.4777649195416,4.95086518422166));
#27908=CARTESIAN_POINT('Ctrl Pts',(-31.598500049601,11.4703968194364,4.96795813428723));
#27909=CARTESIAN_POINT('Ctrl Pts',(-31.7166474940121,11.4605262209518,4.99062508498457));
#27910=CARTESIAN_POINT('Ctrl Pts',(-31.8370362660239,11.4504683713172,5.01372204127766));
#27911=CARTESIAN_POINT('Ctrl Pts',(-31.9560893898572,11.4378120739152,5.04260657014114));
#27912=CARTESIAN_POINT('Ctrl Pts',(-32.0733128635378,11.4224738258393,5.07711450511167));
#27913=CARTESIAN_POINT('Ctrl Pts',(-32.163152626949,11.41071863266,5.10356129615291));
#27914=CARTESIAN_POINT('Ctrl Pts',(-32.2519177179933,11.3973871095325,5.13331061927783));
#27915=CARTESIAN_POINT('Ctrl Pts',(-32.3393857592323,11.3824232903062,5.16627912915032));
#27916=CARTESIAN_POINT('Ctrl Pts',(-32.4793850534024,11.3584725524127,5.219047752371));
#27917=CARTESIAN_POINT('Ctrl Pts',(-32.6155704337176,11.3303376850812,5.28007244007344));
#27918=CARTESIAN_POINT('Ctrl Pts',(-32.7467602549158,11.2979857588007,5.3484126424516));
#27919=CARTESIAN_POINT('Ctrl Pts',(-32.8981892942102,11.2606427616746,5.42729598185089));
#27920=CARTESIAN_POINT('Ctrl Pts',(-33.0429625044899,11.2176785361037,5.5159263629673));
#27921=CARTESIAN_POINT('Ctrl Pts',(-33.1792626377584,11.1689943179435,5.61280374908537));
#27922=CARTESIAN_POINT('Ctrl Pts',(-33.282799048435,11.1320127751963,5.68639382265225));
#27923=CARTESIAN_POINT('Ctrl Pts',(-33.3814462928861,11.0917291827592,5.76474127564139));
#27924=CARTESIAN_POINT('Ctrl Pts',(-33.474407836462,11.0481025616628,5.84717280290056));
#27925=CARTESIAN_POINT('Ctrl Pts',(-33.5358302627105,11.0192771698536,5.9016377376346));
#27926=CARTESIAN_POINT('Ctrl Pts',(-33.5945384654344,10.9892895547735,5.95733345481929));
#27927=CARTESIAN_POINT('Ctrl Pts',(-33.6510314177442,10.9577109032453,6.01486257207092));
#27928=CARTESIAN_POINT('Ctrl Pts',(-33.7049759490101,10.9275567780836,6.06979652643865));
#27929=CARTESIAN_POINT('Ctrl Pts',(-33.7569005837092,10.8959519591392,6.12640235390672));
#27930=CARTESIAN_POINT('Ctrl Pts',(-33.807239768638,10.8624837089529,6.18517967990693));
#27931=CARTESIAN_POINT('Ctrl Pts',(-33.8420919974232,10.8393120363447,6.22587403791129));
#27932=CARTESIAN_POINT('Ctrl Pts',(-33.8761842478221,10.8152463489225,6.26760880092171));
#27933=CARTESIAN_POINT('Ctrl Pts',(-33.9096607013978,10.7901374638712,6.3105414593966));
#27934=CARTESIAN_POINT('Ctrl Pts',(-33.9758931100084,10.7404601009238,6.39548275619247));
#27935=CARTESIAN_POINT('Ctrl Pts',(-34.0363090225637,10.6891510387895,6.4809126865769));
#27936=CARTESIAN_POINT('Ctrl Pts',(-34.0909084390637,10.6361483862253,6.56676080774973));
#27937=CARTESIAN_POINT('Ctrl Pts',(-34.115630943938,10.6121488928174,6.60563266261909));
#27938=CARTESIAN_POINT('Ctrl Pts',(-34.1387959172038,10.5882672441134,6.64384519197078));
#27939=CARTESIAN_POINT('Ctrl Pts',(-34.1608991708523,10.5638733668066,6.68240821037408));
#27940=CARTESIAN_POINT('Ctrl Pts',(-34.1825935762304,10.5399307078907,6.72025792097077));
#27941=CARTESIAN_POINT('Ctrl Pts',(-34.2032651764047,10.5154945835208,6.75844537524371));
#27942=CARTESIAN_POINT('Ctrl Pts',(-34.223382775751,10.4899273921746,6.79789844782233));
#27943=CARTESIAN_POINT('Ctrl Pts',(-34.2280352811117,10.4840145845503,6.80702257980792));
#27944=CARTESIAN_POINT('Ctrl Pts',(-34.2326581564576,10.4780411017129,6.81621428094331));
#27945=CARTESIAN_POINT('Ctrl Pts',(-34.2372572003978,10.4719987212801,6.82548480193958));
#27946=CARTESIAN_POINT('Ctrl Pts',(-34.2566870650782,10.4464711038701,6.86465054395384));
#27947=CARTESIAN_POINT('Ctrl Pts',(-34.2750600716674,10.4202268419957,6.9044275590959));
#27948=CARTESIAN_POINT('Ctrl Pts',(-34.2920469852468,10.3938922755973,6.94384643863036));
#27949=CARTESIAN_POINT('Ctrl Pts',(-34.3092271223809,10.3672581575172,6.98371370191544));
#27950=CARTESIAN_POINT('Ctrl Pts',(-34.3249894539689,10.3405317216853,7.02321454878686));
#27951=CARTESIAN_POINT('Ctrl Pts',(-34.3389933818204,10.3144057106446,7.06137627068701));
#27952=CARTESIAN_POINT('Ctrl Pts',(-34.3430311355361,10.3068727956457,7.07237944322795));
#27953=CARTESIAN_POINT('Ctrl Pts',(-34.3469227056967,10.299390071953,7.0832714805828));
#27954=CARTESIAN_POINT('Ctrl Pts',(-34.3506599281287,10.2919747916331,7.09402952407088));
#27955=CARTESIAN_POINT('Ctrl Pts',(-34.3654172613517,10.2626937508031,7.13651027962354));
#27956=CARTESIAN_POINT('Ctrl Pts',(-34.3790083421857,10.2320408948611,7.18041918774137));
#27957=CARTESIAN_POINT('Ctrl Pts',(-34.3914331706306,10.1999569961636,7.22570946526452));
#27958=CARTESIAN_POINT('Ctrl Pts',(-34.3976455848531,10.1839150468149,7.24835460402609));
#27959=CARTESIAN_POINT('Ctrl Pts',(-34.4035664359783,10.1675152840043,7.27134501205274));
#27960=CARTESIAN_POINT('Ctrl Pts',(-34.4091957240062,10.1507499979578,7.29467439156538));
#27961=CARTESIAN_POINT('Ctrl Pts',(-34.4126060387826,10.1405933134089,7.30880771131758));
#27962=CARTESIAN_POINT('Ctrl Pts',(-34.4162059258583,10.1292799124079,7.32448055502478));
#27963=CARTESIAN_POINT('Ctrl Pts',(-34.4194563664031,10.1186636639247,7.3391174984714));
#27964=CARTESIAN_POINT('Ctrl Pts',(-34.4215713150507,10.1117560401538,7.34864124865926));
#27965=CARTESIAN_POINT('Ctrl Pts',(-34.423538320183,10.1051446046541,7.3577271785419));
#27966=CARTESIAN_POINT('Ctrl Pts',(-34.4252088987983,10.0993496647521,7.36567283749913));
#27967=CARTESIAN_POINT('Ctrl Pts',(-34.4336850426113,10.0699474303711,7.40598734134544));
#27968=CARTESIAN_POINT('Ctrl Pts',(-34.4416590954488,10.0383231334541,7.44884386030834));
#27969=CARTESIAN_POINT('Ctrl Pts',(-34.4491310573107,10.004375657046,7.49416224221931));
#27970=CARTESIAN_POINT('Ctrl Pts',(-34.4528670382416,9.98740191884192,7.5168214331748));
#27971=CARTESIAN_POINT('Ctrl Pts',(-34.4564774964286,9.96984721127902,7.54009589904758));
#27972=CARTESIAN_POINT('Ctrl Pts',(-34.4599624318717,9.95169787784942,7.5639744412582));
#27973=CARTESIAN_POINT('Ctrl Pts',(-34.4617048995933,9.94262321113463,7.57591371236351));
#27974=CARTESIAN_POINT('Ctrl Pts',(-34.4634159866289,9.93339987760537,7.58800398998438));
#27975=CARTESIAN_POINT('Ctrl Pts',(-34.4650956929785,9.92402610913804,7.60024379774402));
#27976=CARTESIAN_POINT('Ctrl Pts',(-34.4662208063714,9.91774730186505,7.60844235675998));
#27977=CARTESIAN_POINT('Ctrl Pts',(-34.4676231516465,9.90966212344636,7.61897017985517));
#27978=CARTESIAN_POINT('Ctrl Pts',(-34.4687173436683,9.90326240728531,7.62727957350781));
#27979=CARTESIAN_POINT('Ctrl Pts',(-34.4692566948061,9.90010784746017,7.63137545506384));
#27980=CARTESIAN_POINT('Ctrl Pts',(-34.469721173352,9.89736368664817,7.63493299557365));
#27981=CARTESIAN_POINT('Ctrl Pts',(-34.4700406699694,9.89545169094337,7.63741028308719));
#27982=CARTESIAN_POINT('Ctrl Pts',(-34.4730979206465,9.87715587858438,7.66111535072587));
#27983=CARTESIAN_POINT('Ctrl Pts',(-34.4765052779658,9.85510583171491,7.68951560275804));
#27984=CARTESIAN_POINT('Ctrl Pts',(-34.4802628093407,9.82917908185892,7.72251504218328));
#27985=CARTESIAN_POINT('Ctrl Pts',(-34.4840168568587,9.80327637041435,7.75548388563696));
#27986=CARTESIAN_POINT('Ctrl Pts',(-34.4881204293941,9.77350402572956,7.79304352192599));
#27987=CARTESIAN_POINT('Ctrl Pts',(-34.4925735941727,9.73970141272728,7.83506326655492));
#27988=CARTESIAN_POINT('Ctrl Pts',(-34.4949495421839,9.72166631743482,7.85748254220371));
#27989=CARTESIAN_POINT('Ctrl Pts',(-34.4974250073895,9.70248329584503,7.88117085678994));
#27990=CARTESIAN_POINT('Ctrl Pts',(-34.5,9.68212365416069,7.90610406872703));
#27991=CARTESIAN_POINT('Origin',(-27.5,0.,0.));
#27992=CARTESIAN_POINT('Origin',(-22.75,0.,0.));
#27993=CARTESIAN_POINT('',(-22.75,-3.06161699786838E-15,25.));
#27994=CARTESIAN_POINT('Origin',(-22.75,0.,0.));
#27995=CARTESIAN_POINT('',(-25.,-2.78607146806023E-15,22.75));
#27996=CARTESIAN_POINT('Origin',(-22.75,-2.78607146806023E-15,22.75));
#27997=CARTESIAN_POINT('Origin',(-25.,0.,0.));
#27998=CARTESIAN_POINT('Origin',(0.,0.,0.));
#27999=CARTESIAN_POINT('',(-13.,-3.06161699786838E-15,25.));
#28000=CARTESIAN_POINT('Origin',(-13.,0.,0.));
#28001=CARTESIAN_POINT('',(0.,-3.06161699786838E-15,25.));
#28002=CARTESIAN_POINT('Origin',(0.,0.,0.));
#28003=CARTESIAN_POINT('',(-20.,-2.75545529808154E-15,22.5));
#28004=CARTESIAN_POINT('Origin',(-20.,0.,0.));
#28005=CARTESIAN_POINT('',(-13.,-2.75545529808154E-15,22.5));
#28006=CARTESIAN_POINT('',(0.,-2.75545529808154E-15,22.5));
#28007=CARTESIAN_POINT('Origin',(-13.,0.,0.));
#28008=CARTESIAN_POINT('Origin',(-44.,0.,0.));
#28009=CARTESIAN_POINT('Ctrl Pts',(-36.1184904636295,3.29830760293365E-8,
-4.12499999999999));
#28010=CARTESIAN_POINT('Ctrl Pts',(-36.1188129792782,-0.0284738922563784,
-4.12500000022766));
#28011=CARTESIAN_POINT('Ctrl Pts',(-36.119137418279,-0.0569608644091503,
-4.12470517782373));
#28012=CARTESIAN_POINT('Ctrl Pts',(-36.1254876843367,-0.611496856226084,
-4.11321455467404));
#28013=CARTESIAN_POINT('Ctrl Pts',(-36.1320388503183,-1.13062218918054,
-4.00176801844617));
#28014=CARTESIAN_POINT('Ctrl Pts',(-36.1457516055008,-2.11795055176676,
-3.58174714378506));
#28015=CARTESIAN_POINT('Ctrl Pts',(-36.1527912778546,-2.57357591918388,
-3.26976117732126));
#28016=CARTESIAN_POINT('Ctrl Pts',(-36.165934186153,-3.32415021752054,-2.49909010546225));
#28017=CARTESIAN_POINT('Ctrl Pts',(-36.1715529781619,-3.61689552156258,
-2.05267925260612));
#28018=CARTESIAN_POINT('Ctrl Pts',(-36.1843221264338,-4.0189975245572,-1.07072393112184));
#28019=CARTESIAN_POINT('Ctrl Pts',(-36.1911232640831,-4.12346679901638,
-0.543881494992523));
#28020=CARTESIAN_POINT('Ctrl Pts',(-36.2049491490745,-4.12653977793352,
0.534433978155843));
#28021=CARTESIAN_POINT('Ctrl Pts',(-36.2118384570041,-4.01959947188852,
1.07553630532412));
#28022=CARTESIAN_POINT('Ctrl Pts',(-36.2243033575539,-3.61049936724165,
2.0620880236769));
#28023=CARTESIAN_POINT('Ctrl Pts',(-36.2300451849934,-3.3209633622173,2.50182336289408));
#28024=CARTESIAN_POINT('Ctrl Pts',(-36.2432508971558,-2.58193474564445,
3.26173128216171));
#28025=CARTESIAN_POINT('Ctrl Pts',(-36.2502136603053,-2.13480494949125,
3.57041793481763));
#28026=CARTESIAN_POINT('Ctrl Pts',(-36.2639684640228,-1.14000541154513,
4.00177987603652));
#28027=CARTESIAN_POINT('Ctrl Pts',(-36.2704812921315,-0.60079422594595,
4.11738773792091));
#28028=CARTESIAN_POINT('Ctrl Pts',(-36.2825196776631,0.469593642929444,
4.13159746634345));
#28029=CARTESIAN_POINT('Ctrl Pts',(-36.2889803312695,0.990488073958131,
4.03850712175553));
#28030=CARTESIAN_POINT('Ctrl Pts',(-36.3025946858657,1.9884930745957,3.65490487200752));
#28031=CARTESIAN_POINT('Ctrl Pts',(-36.3096317543173,2.45329967538008,3.36061865545876));
#28032=CARTESIAN_POINT('Ctrl Pts',(-36.3229459347788,3.23315456097611,2.61657770970833));
#28033=CARTESIAN_POINT('Ctrl Pts',(-36.3286722456059,3.5438698456838,2.17732672202478));
#28034=CARTESIAN_POINT('Ctrl Pts',(-36.3413023232013,3.97983419336367,1.20740145021164));
#28035=CARTESIAN_POINT('Ctrl Pts',(-36.3480384347988,4.10194551352598,0.686247137589298));
#28036=CARTESIAN_POINT('Ctrl Pts',(-36.3619189074336,4.14293964986017,-0.395001950570159));
#28037=CARTESIAN_POINT('Ctrl Pts',(-36.368928880632,4.05303669850736,-0.944921243939712));
#28038=CARTESIAN_POINT('Ctrl Pts',(-36.3816408239285,3.67252141824346,-1.94974415955186));
#28039=CARTESIAN_POINT('Ctrl Pts',(-36.3872785848625,3.39612511880639,-2.39901076688027));
#28040=CARTESIAN_POINT('Ctrl Pts',(-36.4003710697463,2.68100395729819,-3.180522530576));
#28041=CARTESIAN_POINT('Ctrl Pts',(-36.4072989140441,2.24502112269832,-3.50191138006792));
#28042=CARTESIAN_POINT('Ctrl Pts',(-36.4210898632463,1.26593074560354,-3.96373034594873));
#28043=CARTESIAN_POINT('Ctrl Pts',(-36.4278135140083,0.730737603887081,
-4.09631201729583));
#28044=CARTESIAN_POINT('Ctrl Pts',(-36.4346052355924,0.123501653108671,
-4.12361452133081));
#28045=CARTESIAN_POINT('Ctrl Pts',(-36.4352913126543,0.0617259448598127,
-4.12499999999999));
#28046=CARTESIAN_POINT('Ctrl Pts',(-36.4359904640031,3.27860210979314E-14,
-4.12499999999999));
#28047=CARTESIAN_POINT('Ctrl Pts',(-36.3566154631359,-4.99089713584757E-13,
-4.12499999999999));
#28048=CARTESIAN_POINT('Ctrl Pts',(-36.356350447845,0.0233973935143799,
-4.12499999999999));
#28049=CARTESIAN_POINT('Ctrl Pts',(-36.3560865337059,0.0468034160332337,
-4.12480093196674));
#28050=CARTESIAN_POINT('Ctrl Pts',(-36.3496955247249,0.616200357154302,
-4.11510727677789));
#28051=CARTESIAN_POINT('Ctrl Pts',(-36.343151671704,1.15495332093977,-3.9974884183394));
#28052=CARTESIAN_POINT('Ctrl Pts',(-36.3293919969298,2.14793688048322,-3.562503756747));
#28053=CARTESIAN_POINT('Ctrl Pts',(-36.3224330248351,2.59376818274409,-3.25229675530295));
#28054=CARTESIAN_POINT('Ctrl Pts',(-36.3092405211388,3.329980523612,-2.48982485883441));
#28055=CARTESIAN_POINT('Ctrl Pts',(-36.3035136276204,3.61796642737089,-2.0489783562903));
#28056=CARTESIAN_POINT('Ctrl Pts',(-36.2910270965324,4.0234975201098,-1.06086408272591));
#28057=CARTESIAN_POINT('Ctrl Pts',(-36.2841318684387,4.1284637457095,-0.519368917559876));
#28058=CARTESIAN_POINT('Ctrl Pts',(-36.2703067656381,4.12145458755141,0.558748090084849));
#28059=CARTESIAN_POINT('Ctrl Pts',(-36.2635120490944,4.01513553202157,1.08502508246555));
#28060=CARTESIAN_POINT('Ctrl Pts',(-36.2507572006762,3.60950704474773,2.06574186393406));
#28061=CARTESIAN_POINT('Ctrl Pts',(-36.2451303961666,3.31491499256384,2.5114079653395));
#28062=CARTESIAN_POINT('Ctrl Pts',(-36.2319694875181,2.5613008089251,3.2793506876566));
#28063=CARTESIAN_POINT('Ctrl Pts',(-36.2249296693748,2.10469647472789,3.5895196928067));
#28064=CARTESIAN_POINT('Ctrl Pts',(-36.2112263289609,1.11620480638802,4.00578944532168));
#28065=CARTESIAN_POINT('Ctrl Pts',(-36.2046841781791,0.596867108969412,
4.11533966572925));
#28066=CARTESIAN_POINT('Ctrl Pts',(-36.1924184950835,-0.476214249019286,
4.13380553048062));
#28067=CARTESIAN_POINT('Ctrl Pts',(-36.1861212783578,-1.01984834863037,
4.03423470121718));
#28068=CARTESIAN_POINT('Ctrl Pts',(-36.1723992977249,-2.02953298946384,
3.63152228096813));
#28069=CARTESIAN_POINT('Ctrl Pts',(-36.1654096344374,-2.48679250804523,
3.33508947972833));
#28070=CARTESIAN_POINT('Ctrl Pts',(-36.1521006902102,-3.24810574947604,
2.59565866040361));
#28071=CARTESIAN_POINT('Ctrl Pts',(-36.1462156604452,-3.54994049759374,
2.16461282875544));
#28072=CARTESIAN_POINT('Ctrl Pts',(-36.1339228823,-3.98705269692777,1.1905085008082));
#28073=CARTESIAN_POINT('Ctrl Pts',(-36.1270834397453,-4.10947705763902,
0.652754971315038));
#28074=CARTESIAN_POINT('Ctrl Pts',(-36.1132578692447,-4.13743266360497,
-0.426619513520434));
#28075=CARTESIAN_POINT('Ctrl Pts',(-36.1064090845789,-4.04761502808193,
-0.957690076385819));
#28076=CARTESIAN_POINT('Ctrl Pts',(-36.0935288802234,-3.67327189816729,
-1.9492771637618));
#28077=CARTESIAN_POINT('Ctrl Pts',(-36.0879476338471,-3.39487095018637,
-2.40155343925716));
#28078=CARTESIAN_POINT('Ctrl Pts',(-36.0749475495251,-2.6681375583289,-3.19334772538381));
#28079=CARTESIAN_POINT('Ctrl Pts',(-36.067912310006,-2.22039104239074,-3.51941561244037));
#28080=CARTESIAN_POINT('Ctrl Pts',(-36.0541320734522,-1.24261636540952,
-3.96860920734908));
#28081=CARTESIAN_POINT('Ctrl Pts',(-36.0475132450743,-0.725382649545967,
-4.09484826686876));
#28082=CARTESIAN_POINT('Ctrl Pts',(-36.0406230669347,-0.132256996684131,
-4.12341124761089));
#28083=CARTESIAN_POINT('Ctrl Pts',(-36.0398641502892,-0.0660993102846563,
-4.12499999999999));
#28084=CARTESIAN_POINT('Ctrl Pts',(-36.0391154631359,3.30485893395058E-14,
-4.12499999999999));
#28085=CARTESIAN_POINT('Origin',(-36.,-4.40872847693047E-15,0.));
#28086=CARTESIAN_POINT('Ctrl Pts',(-36.,2.8677394674816,-2.96507931540595));
#28087=CARTESIAN_POINT('Ctrl Pts',(-36.,2.58211488762459,-3.25359758419502));
#28088=CARTESIAN_POINT('Ctrl Pts',(-36.,2.2556303657079,-3.49857150536326));
#28089=CARTESIAN_POINT('Ctrl Pts',(-36.,1.53011798561339,-3.89209437568881));
#28090=CARTESIAN_POINT('Ctrl Pts',(-36.0000000000009,1.13324515947091,-4.03492093053112));
#28091=CARTESIAN_POINT('Ctrl Pts',(-36.0000000000009,0.144604455351344,
-4.22907725009426));
#28092=CARTESIAN_POINT('Ctrl Pts',(-36.,-0.418973144257557,-4.2124931411291));
#28093=CARTESIAN_POINT('Ctrl Pts',(-36.,-1.46036865006272,-3.99898257282591));
#28094=CARTESIAN_POINT('Ctrl Pts',(-36.,-1.96289610596394,-3.79090818666882));
#28095=CARTESIAN_POINT('Ctrl Pts',(-36.,-2.75244104700568,-3.27033011728567));
#28096=CARTESIAN_POINT('Ctrl Pts',(-36.,-3.05797105898633,-2.99870283738677));
#28097=CARTESIAN_POINT('Ctrl Pts',(-36.,-3.60220512633872,-2.35292484380394));
#28098=CARTESIAN_POINT('Ctrl Pts',(-36.,-3.83066360686449,-1.97559567188751));
#28099=CARTESIAN_POINT('Ctrl Pts',(-36.,-3.99810942017504,-1.57418469260505));
#28100=CARTESIAN_POINT('Ctrl Pts',(-36.,-3.96679264203453,1.65151219106172));
#28101=CARTESIAN_POINT('Ctrl Pts',(-36.,-3.78888208787887,2.05652148838597));
#28102=CARTESIAN_POINT('Ctrl Pts',(-36.,-3.54982596258504,2.4323494533105));
#28103=CARTESIAN_POINT('Ctrl Pts',(-36.,-2.98666653493592,3.06859799774672));
#28104=CARTESIAN_POINT('Ctrl Pts',(-36.,-2.67569031699454,3.332187707082));
#28105=CARTESIAN_POINT('Ctrl Pts',(-36.,-1.88238697005194,3.82949480800279));
#28106=CARTESIAN_POINT('Ctrl Pts',(-36.,-1.38380077745684,4.02451205440474));
#28107=CARTESIAN_POINT('Ctrl Pts',(-36.,-0.364900368386679,4.21598353592192));
#28108=CARTESIAN_POINT('Ctrl Pts',(-35.9999999999974,0.197924631338814,
4.22987474907417));
#28109=CARTESIAN_POINT('Ctrl Pts',(-35.9999999999974,1.19242231635065,4.01726970897806));
#28110=CARTESIAN_POINT('Ctrl Pts',(-36.,1.58187588327058,3.87073756876392));
#28111=CARTESIAN_POINT('Ctrl Pts',(-36.,2.30197555597678,3.46876308718649));
#28112=CARTESIAN_POINT('Ctrl Pts',(-36.,2.62903433812351,3.21631429554064));
#28113=CARTESIAN_POINT('Ctrl Pts',(-36.,2.91366312592486,2.91996441564374));
#28114=CARTESIAN_POINT('Origin',(-20.,8.,0.));
#28115=CARTESIAN_POINT('Origin',(-13.,22.5,0.));
#28116=CARTESIAN_POINT('Origin',(-25.,22.75,0.));
#28117=CARTESIAN_POINT('Origin',(-44.,11.5,0.));
#28118=CARTESIAN_POINT('Ctrl Pts',(-27.4978820065166,9.67657286048411,7.93453028901309));
#28119=CARTESIAN_POINT('Ctrl Pts',(-27.5051002838282,9.73192148554358,7.86702396692179));
#28120=CARTESIAN_POINT('Ctrl Pts',(-27.5115777941627,9.77905015687421,7.80813914050018));
#28121=CARTESIAN_POINT('Ctrl Pts',(-27.5198997026027,9.8361990199015,7.73581472965319));
#28122=CARTESIAN_POINT('Ctrl Pts',(-27.5223343384609,9.85237966752398,7.71518001660921));
#28123=CARTESIAN_POINT('Ctrl Pts',(-27.5257607197538,9.8743467249716,7.68701758369407));
#28124=CARTESIAN_POINT('Ctrl Pts',(-27.5268652514357,9.8812849948035,7.67809495754876));
#28125=CARTESIAN_POINT('Ctrl Pts',(-27.5289991239681,9.89440105342999,7.66118549048045));
#28126=CARTESIAN_POINT('Ctrl Pts',(-27.5293642597536,9.89669372379413,7.65823253102818));
#28127=CARTESIAN_POINT('Ctrl Pts',(-27.5376440122518,9.9451242809251,7.59548188702668));
#28128=CARTESIAN_POINT('Ctrl Pts',(-27.5447308790556,9.98143874139635,7.54764313910302));
#28129=CARTESIAN_POINT('Ctrl Pts',(-27.5560557764691,10.0324327883853,7.4795666351035));
#28130=CARTESIAN_POINT('Ctrl Pts',(-27.5599465084749,10.0488510371663,7.45748786474674));
#28131=CARTESIAN_POINT('Ctrl Pts',(-27.5679595048892,10.0805539119409,7.41457788740912));
#28132=CARTESIAN_POINT('Ctrl Pts',(-27.5712462791805,10.0929346338891,7.39772849754879));
#28133=CARTESIAN_POINT('Ctrl Pts',(-27.5966138828154,10.1811045843937,7.27683035868852));
#28134=CARTESIAN_POINT('Ctrl Pts',(-27.6197351110962,10.2422025103862,7.19039294558005));
#28135=CARTESIAN_POINT('Ctrl Pts',(-27.6806178014129,10.3646680115295,7.0127113149185));
#28136=CARTESIAN_POINT('Ctrl Pts',(-27.7200563355264,10.4272692165682,6.91921499537165));
#28137=CARTESIAN_POINT('Ctrl Pts',(-27.8481422012966,10.5963833319316,6.65973840660726));
#28138=CARTESIAN_POINT('Ctrl Pts',(-27.9606936772239,10.7049090095097,6.48342500331331));
#28139=CARTESIAN_POINT('Ctrl Pts',(-28.2199472395629,10.8992663187099,6.15108692747109));
#28140=CARTESIAN_POINT('Ctrl Pts',(-28.3639945150494,10.9842519347326,5.99712178198714));
#28141=CARTESIAN_POINT('Ctrl Pts',(-29.1735457901792,11.364545034686,5.27853837366088));
#28142=CARTESIAN_POINT('Ctrl Pts',(-30.0801163558429,11.5024937103589,4.92802793068232));
#28143=CARTESIAN_POINT('Ctrl Pts',(-31.4601577094634,11.5025432544128,4.92791228792853));
#28144=CARTESIAN_POINT('Ctrl Pts',(-31.9150359953972,11.4675795904092,5.01182201720196));
#28145=CARTESIAN_POINT('Ctrl Pts',(-32.7637355230674,11.3222269507453,5.33206512247338));
#28146=CARTESIAN_POINT('Ctrl Pts',(-33.1530450432979,11.2111961005192,5.56831023126238));
#28147=CARTESIAN_POINT('Ctrl Pts',(-33.635089233044,10.9847259259335,5.99622057363153));
#28148=CARTESIAN_POINT('Ctrl Pts',(-33.7771958841765,10.90143170776,6.14739164137836));
#28149=CARTESIAN_POINT('Ctrl Pts',(-33.9758931100084,10.7522362163205,6.40249492720256));
#28150=CARTESIAN_POINT('Ctrl Pts',(-34.0363090225637,10.700870897617,6.48801852514955));
#28151=CARTESIAN_POINT('Ctrl Pts',(-34.1455078555637,10.5947493655584,6.65990301965054));
#28152=CARTESIAN_POINT('Ctrl Pts',(-34.1925105204025,10.5423346581866,6.74267144025955));
#28153=CARTESIAN_POINT('Ctrl Pts',(-34.282003880393,10.4246263193092,6.92326543614069));
#28154=CARTESIAN_POINT('Ctrl Pts',(-34.3211452616827,10.3618854668815,7.01675293455816));
#28155=CARTESIAN_POINT('Ctrl Pts',(-34.3654172613517,10.2739460309433,7.14433493217967));
#28156=CARTESIAN_POINT('Ctrl Pts',(-34.3790083421857,10.2432595664254,7.18829198314837));
#28157=CARTESIAN_POINT('Ctrl Pts',(-34.3976455848531,10.1950809519674,7.25630188556257));
#28158=CARTESIAN_POINT('Ctrl Pts',(-34.4035664359783,10.1786632080371,7.27931750086111));
#28159=CARTESIAN_POINT('Ctrl Pts',(-34.4148250120342,10.1450958721665,7.32602741774418));
#28160=CARTESIAN_POINT('Ctrl Pts',(-34.4209708268918,10.1251400861266,7.35356939689983));
#28161=CARTESIAN_POINT('Ctrl Pts',(-34.4336850426113,10.0809883785116,7.41410745545032));
#28162=CARTESIAN_POINT('Ctrl Pts',(-34.4416590954488,10.0493294079059,7.45701096339767));
#28163=CARTESIAN_POINT('Ctrl Pts',(-34.4528670382416,9.99835236197048,7.52506306861516));
#28164=CARTESIAN_POINT('Ctrl Pts',(-34.4564774964286,9.98077840697682,7.54836305320812));
#28165=CARTESIAN_POINT('Ctrl Pts',(-34.4617048995933,9.95352455774178,7.58422013809147));
#28166=CARTESIAN_POINT('Ctrl Pts',(-34.4634159866289,9.94429111151353,7.59632367180222));
#28167=CARTESIAN_POINT('Ctrl Pts',(-34.4667753993281,9.92552301929947,7.6208301273986));
#28168=CARTESIAN_POINT('Ctrl Pts',(-34.469073004422,9.91209856492485,7.6382729004231));
#28169=CARTESIAN_POINT('Ctrl Pts',(-34.47820638366,9.85738083779885,7.70916821772884));
#28170=CARTESIAN_POINT('Ctrl Pts',(-34.4888697183811,9.7817723769294,7.80619779242128));
#28171=CARTESIAN_POINT('Ctrl Pts',(-34.5020319587248,9.67657706129138,7.93452721162802));
#28172=CARTESIAN_POINT('Ctrl Pts',(-27.4978820071632,3.47975094352918,2.85330246801448));
#28173=CARTESIAN_POINT('Ctrl Pts',(-27.5051002818624,3.49965461851457,2.82902681724709));
#28174=CARTESIAN_POINT('Ctrl Pts',(-27.5115777941627,3.51660236362271,2.80785149032865));
#28175=CARTESIAN_POINT('Ctrl Pts',(-27.5198997026027,3.53715342160648,2.78184321855869));
#28176=CARTESIAN_POINT('Ctrl Pts',(-27.5223343384609,3.54297207503001,2.77442285773641));
#28177=CARTESIAN_POINT('Ctrl Pts',(-27.5257607197538,3.55087155451962,2.7642954857968));
#28178=CARTESIAN_POINT('Ctrl Pts',(-27.5268652514357,3.55336659603172,2.7610868584057));
#28179=CARTESIAN_POINT('Ctrl Pts',(-27.5289991239681,3.55808320572565,2.75500611734127));
#28180=CARTESIAN_POINT('Ctrl Pts',(-27.5293642597536,3.55890766310057,2.75394421623401));
#28181=CARTESIAN_POINT('Ctrl Pts',(-27.5376440122518,3.5763235684233,2.73137872577486));
#28182=CARTESIAN_POINT('Ctrl Pts',(-27.5447308790556,3.58938245609422,2.71417563842768));
#28183=CARTESIAN_POINT('Ctrl Pts',(-27.5560557764691,3.60772020703069,2.6896949382542));
#28184=CARTESIAN_POINT('Ctrl Pts',(-27.5599465084749,3.61362430318968,2.68175528616356));
#28185=CARTESIAN_POINT('Ctrl Pts',(-27.5679595048892,3.62502483827003,2.66632461290719));
#28186=CARTESIAN_POINT('Ctrl Pts',(-27.5712462791805,3.62947701668899,2.66026547595033));
#28187=CARTESIAN_POINT('Ctrl Pts',(-27.5966138828154,3.66118343514184,2.61678981378955));
#28188=CARTESIAN_POINT('Ctrl Pts',(-27.6197351110962,3.68315459875289,2.5857064256929));
#28189=CARTESIAN_POINT('Ctrl Pts',(-27.6806178014129,3.72719389335453,2.52181109513081));
#28190=CARTESIAN_POINT('Ctrl Pts',(-27.7200563355264,3.74970564470802,2.48818928390845));
#28191=CARTESIAN_POINT('Ctrl Pts',(-27.8481422012966,3.81052004777055,2.39488001862033));
#28192=CARTESIAN_POINT('Ctrl Pts',(-27.9606936772239,3.84954650209512,2.33147671044463));
#28193=CARTESIAN_POINT('Ctrl Pts',(-28.2199472395629,3.91943850202933,2.21196603770235));
#28194=CARTESIAN_POINT('Ctrl Pts',(-28.3639945150494,3.94999981559095,2.1565992908467));
#28195=CARTESIAN_POINT('Ctrl Pts',(-29.1735457901792,4.08675538926246,1.89819258757359));
#28196=CARTESIAN_POINT('Ctrl Pts',(-30.0801163558429,4.13636252197452,1.77214702767979));
#28197=CARTESIAN_POINT('Ctrl Pts',(-31.4601577094634,4.13638033829966,1.77210544188415));
#28198=CARTESIAN_POINT('Ctrl Pts',(-31.9150359953972,4.1238072047638,1.80227986041768));
#28199=CARTESIAN_POINT('Ctrl Pts',(-32.7637355230674,4.07153756425668,1.91744111257055));
#28200=CARTESIAN_POINT('Ctrl Pts',(-33.1530450432979,4.03161023552061,2.00239620479673));
#28201=CARTESIAN_POINT('Ctrl Pts',(-33.635089233044,3.9501702655376,2.15627521116793));
#28202=CARTESIAN_POINT('Ctrl Pts',(-33.7771958841765,3.92021718831577,2.21063719168975));
#28203=CARTESIAN_POINT('Ctrl Pts',(-33.9758931100084,3.86656563633256,2.30237379222929));
#28204=CARTESIAN_POINT('Ctrl Pts',(-34.0363090225637,3.84809437396421,2.33312856716768));
#28205=CARTESIAN_POINT('Ctrl Pts',(-34.1455078555637,3.80993246411797,2.39493921441212));
#28206=CARTESIAN_POINT('Ctrl Pts',(-34.1925105204025,3.79108383558294,2.42470321182269));
#28207=CARTESIAN_POINT('Ctrl Pts',(-34.282003880393,3.74875524373872,2.48964584557381));
#28208=CARTESIAN_POINT('Ctrl Pts',(-34.3211452616827,3.72619327438553,2.5232644846676));
#28209=CARTESIAN_POINT('Ctrl Pts',(-34.3654172613517,3.6945697502891,2.56914370066447));
#28210=CARTESIAN_POINT('Ctrl Pts',(-34.3790083421857,3.68353472214999,2.58495090758689));
#28211=CARTESIAN_POINT('Ctrl Pts',(-34.3976455848531,3.66620941685335,2.60940765744939));
#28212=CARTESIAN_POINT('Ctrl Pts',(-34.4035664359783,3.66030550224154,2.61768420433899));
#28213=CARTESIAN_POINT('Ctrl Pts',(-34.4148250120342,3.64823449628808,2.63448135758808));
#28214=CARTESIAN_POINT('Ctrl Pts',(-34.4209708268918,3.64105828149931,2.64438561080735));
#28215=CARTESIAN_POINT('Ctrl Pts',(-34.4336850426113,3.6251810749336,2.66615544288436));
#28216=CARTESIAN_POINT('Ctrl Pts',(-34.4416590954488,3.61379632804348,2.681583789711));
#28217=CARTESIAN_POINT('Ctrl Pts',(-34.4528670382416,3.59546469078309,2.70605571594293));
#28218=CARTESIAN_POINT('Ctrl Pts',(-34.4564774964286,3.58914499606044,2.71443452365713));
#28219=CARTESIAN_POINT('Ctrl Pts',(-34.4617048995933,3.57934435600846,2.72732893645086));
#28220=CARTESIAN_POINT('Ctrl Pts',(-34.4634159866289,3.57602395593793,2.73168143639438));
#28221=CARTESIAN_POINT('Ctrl Pts',(-34.4667753993281,3.56927484264146,2.74049409798132));
#28222=CARTESIAN_POINT('Ctrl Pts',(-34.469073004422,3.56444733207276,2.74676661891762));
#28223=CARTESIAN_POINT('Ctrl Pts',(-34.47820638366,3.54477052446296,2.77226098047704));
#28224=CARTESIAN_POINT('Ctrl Pts',(-34.4888697350336,3.51758124217551,2.80715342844052));
#28225=CARTESIAN_POINT('Ctrl Pts',(-34.5020319559861,3.47975246018584,2.85330135399401));
#28226=CARTESIAN_POINT('',(-27.5,6.19655913866284,5.0599066039853));
#28227=CARTESIAN_POINT('',(-34.5,6.19655913866284,5.0599066039853));
#28228=CARTESIAN_POINT('Origin',(-34.5,0.,0.));
#28229=CARTESIAN_POINT('',(-34.5,-2.47065947129021,7.60893171062298));
#28230=CARTESIAN_POINT('Ctrl Pts',(-34.5021179935156,-3.84034921836418,
11.9098510115161));
#28231=CARTESIAN_POINT('Ctrl Pts',(-34.494899716168,-3.92343148484306,11.8830571522946));
#28232=CARTESIAN_POINT('Ctrl Pts',(-34.4884222058122,-3.99493511172526,
11.8590620314241));
#28233=CARTESIAN_POINT('Ctrl Pts',(-34.4801002973656,-4.08213937064346,
11.8291918089636));
#28234=CARTESIAN_POINT('Ctrl Pts',(-34.4776656615101,-4.10691485581785,
11.8206022762278));
#28235=CARTESIAN_POINT('Ctrl Pts',(-34.4742392802251,-4.1406307585753,11.8088161769966));
#28236=CARTESIAN_POINT('Ctrl Pts',(-34.4731347485465,-4.15129480472915,
11.8050703841133));
#28237=CARTESIAN_POINT('Ctrl Pts',(-34.471000876022,-4.17147688887322,11.7979538859599));
#28238=CARTESIAN_POINT('Ctrl Pts',(-34.4706357402539,-4.17500317883281,
11.796712280233));
#28239=CARTESIAN_POINT('Ctrl Pts',(-34.4623559877182,-4.2496942586282,11.770171654287));
#28240=CARTESIAN_POINT('Ctrl Pts',(-34.4552691208995,-4.3061254359688,11.7496093567904));
#28241=CARTESIAN_POINT('Ctrl Pts',(-34.4439442234859,-4.38585513082339,
11.7199786466456));
#28242=CARTESIAN_POINT('Ctrl Pts',(-34.4400534914838,-4.41161216089477,
11.710303606902));
#28243=CARTESIAN_POINT('Ctrl Pts',(-34.4320404950846,-4.46149769348112,
11.6913887436455));
#28244=CARTESIAN_POINT('Ctrl Pts',(-34.4287537208257,-4.48102899522492,
11.6839246657677));
#28245=CARTESIAN_POINT('Ctrl Pts',(-34.4033861171601,-4.62061175533369,
11.6300084968999));
#28246=CARTESIAN_POINT('Ctrl Pts',(-34.3802648888803,-4.71877671883352,
11.5904102281741));
#28247=CARTESIAN_POINT('Ctrl Pts',(-34.3193821986106,-4.91793563737523,
11.507318195227));
#28248=CARTESIAN_POINT('Ctrl Pts',(-34.2799436644392,-5.02118603476733,
11.4625987574891));
#28249=CARTESIAN_POINT('Ctrl Pts',(-34.1518577987722,-5.30384788925113,
11.3359892789864));
#28250=CARTESIAN_POINT('Ctrl Pts',(-34.0393063228094,-5.49054572845524,
11.2465009795587));
#28251=CARTESIAN_POINT('Ctrl Pts',(-33.7800527604038,-5.83387687678551,
11.0722968378733));
#28252=CARTESIAN_POINT('Ctrl Pts',(-33.6360054850864,-5.98868389780719,
10.9888545995394));
#28253=CARTESIAN_POINT('Ctrl Pts',(-32.8264542092776,-6.69744947821504,
10.590562860345));
#28254=CARTESIAN_POINT('Ctrl Pts',(-31.9198836441155,-7.00319127556429,
10.3705415868347));
#28255=CARTESIAN_POINT('Ctrl Pts',(-30.5398422905574,-7.00329553722076,
10.3704711782771));
#28256=CARTESIAN_POINT('Ctrl Pts',(-30.08496400456,-6.92847222075559,10.4220926058383));
#28257=CARTESIAN_POINT('Ctrl Pts',(-29.2362644769754,-6.63289122824282,
10.6126573275853));
#28258=CARTESIAN_POINT('Ctrl Pts',(-28.8469549569745,-6.41164166105415,
10.7511789144381));
#28259=CARTESIAN_POINT('Ctrl Pts',(-28.3649107668198,-5.98957031134368,
10.9883534856232));
#28260=CARTESIAN_POINT('Ctrl Pts',(-28.2228041159262,-5.83769802696752,
11.0703621901657));
#28261=CARTESIAN_POINT('Ctrl Pts',(-28.0241068899402,-5.57415098904807,
11.2040780834347));
#28262=CARTESIAN_POINT('Ctrl Pts',(-27.9636909773592,-5.48466374516304,
11.2481770059251));
#28263=CARTESIAN_POINT('Ctrl Pts',(-27.8544921443592,-5.30238496198931,
11.3352430970402));
#28264=CARTESIAN_POINT('Ctrl Pts',(-27.8074894795624,-5.21350699011682,
11.3764574039751));
#28265=CARTESIAN_POINT('Ctrl Pts',(-27.717996119642,-5.01677113301965,11.4645735027238));
#28266=CARTESIAN_POINT('Ctrl Pts',(-27.678854738298,-4.91340809804618,11.5092099224669));
#28267=CARTESIAN_POINT('Ctrl Pts',(-27.6345827386579,-4.77040068831785,
11.5688705562283));
#28268=CARTESIAN_POINT('Ctrl Pts',(-27.6209916578288,-4.72080287780926,
11.5892160378951));
#28269=CARTESIAN_POINT('Ctrl Pts',(-27.6023544151614,-4.64347640529298,
11.6203149505103));
#28270=CARTESIAN_POINT('Ctrl Pts',(-27.596433564035,-4.61721261685308,11.6307779462829));
#28271=CARTESIAN_POINT('Ctrl Pts',(-27.5851749879742,-4.56370229244711,
11.6518783623449));
#28272=CARTESIAN_POINT('Ctrl Pts',(-27.579029173103,-4.53201332813435,11.6642316436317));
#28273=CARTESIAN_POINT('Ctrl Pts',(-27.566314957399,-4.46211766449134,11.6912284213788));
#28274=CARTESIAN_POINT('Ctrl Pts',(-27.5583409045667,-4.4122725480453,11.710161613854));
#28275=CARTESIAN_POINT('Ctrl Pts',(-27.5471329617739,-4.33257035622456,
11.7397810138477));
#28276=CARTESIAN_POINT('Ctrl Pts',(-27.5435225035856,-4.305180495978,11.7498571605463));
#28277=CARTESIAN_POINT('Ctrl Pts',(-27.538295100417,-4.26285387292635,11.7652506597461));
#28278=CARTESIAN_POINT('Ctrl Pts',(-27.5365840133798,-4.24853802456432,
11.7704283564838));
#28279=CARTESIAN_POINT('Ctrl Pts',(-27.5332246006767,-4.21949100363759,
11.7808724087611));
#28280=CARTESIAN_POINT('Ctrl Pts',(-27.5309269955758,-4.19876090805562,
11.7882703439938));
#28281=CARTESIAN_POINT('Ctrl Pts',(-27.521793616354,-4.11437437864175,11.8182551616966));
#28282=CARTESIAN_POINT('Ctrl Pts',(-27.5111302816239,-3.99827490007513,
11.8589035174418));
#28283=CARTESIAN_POINT('Ctrl Pts',(-27.4979680412483,-3.84035441638973,
11.9098506982947));
#28284=CARTESIAN_POINT('Ctrl Pts',(-34.502117992869,-1.38101154484016,4.2828505362653));
#28285=CARTESIAN_POINT('Ctrl Pts',(-34.4948997181338,-1.41088839229903,
4.2732153147342));
#28286=CARTESIAN_POINT('Ctrl Pts',(-34.4884222058122,-1.43660151352823,
4.26458652941962));
#28287=CARTESIAN_POINT('Ctrl Pts',(-34.4801002973656,-1.46796066376331,
4.25384502659264));
#28288=CARTESIAN_POINT('Ctrl Pts',(-34.4776656615101,-1.47687006992499,
4.25075618149666));
#28289=CARTESIAN_POINT('Ctrl Pts',(-34.4742392802251,-1.4889945013805,4.24651783280745));
#28290=CARTESIAN_POINT('Ctrl Pts',(-34.4731347485465,-1.49282935336596,
4.24517082426415));
#28291=CARTESIAN_POINT('Ctrl Pts',(-34.471000876022,-1.50008694624711,4.24261169082837));
#28292=CARTESIAN_POINT('Ctrl Pts',(-34.4706357402539,-1.50135502028371,
4.24216520230811));
#28293=CARTESIAN_POINT('Ctrl Pts',(-34.4623559877182,-1.52821435974236,
4.23262104143));
#28294=CARTESIAN_POINT('Ctrl Pts',(-34.4552691208995,-1.54850733384844,
4.2252267216528));
#28295=CARTESIAN_POINT('Ctrl Pts',(-34.4439442234859,-1.57717858809862,
4.21457134882434));
#28296=CARTESIAN_POINT('Ctrl Pts',(-34.4400534914838,-1.58644096341879,
4.21109214920023));
#28297=CARTESIAN_POINT('Ctrl Pts',(-34.4320404950845,-1.60438008623618,
4.20429025619756));
#28298=CARTESIAN_POINT('Ctrl Pts',(-34.4287537208257,-1.61140365404432,
4.20160613110506));
#28299=CARTESIAN_POINT('Ctrl Pts',(-34.4033861171601,-1.66159841286434,
4.18221756842935));
#28300=CARTESIAN_POINT('Ctrl Pts',(-34.3802648888803,-1.69689909515212,
4.16797780452988));
#28301=CARTESIAN_POINT('Ctrl Pts',(-34.3193821986106,-1.76851778126542,
4.13809743427216));
#28302=CARTESIAN_POINT('Ctrl Pts',(-34.2799436644392,-1.80564721466486,
4.12201606870759));
#28303=CARTESIAN_POINT('Ctrl Pts',(-34.1518577987722,-1.90729403410288,
4.07648657614834));
#28304=CARTESIAN_POINT('Ctrl Pts',(-34.0393063228094,-1.97443164482047,
4.04430607188342));
#28305=CARTESIAN_POINT('Ctrl Pts',(-33.7800527604038,-2.0978954892982,3.98166126624602));
#28306=CARTESIAN_POINT('Ctrl Pts',(-33.6360054850864,-2.15356497941127,
3.95165496012834));
#28307=CARTESIAN_POINT('Ctrl Pts',(-32.8264542092776,-2.40844113561269,
3.80842697285189));
#28308=CARTESIAN_POINT('Ctrl Pts',(-31.9198836441155,-2.51838763450115,
3.72930606457842));
#28309=CARTESIAN_POINT('Ctrl Pts',(-30.5398422905574,-2.5184251275891,3.72928074525843));
#28310=CARTESIAN_POINT('Ctrl Pts',(-30.08496400456,-2.49151823506772,3.74784410583648));
#28311=CARTESIAN_POINT('Ctrl Pts',(-29.2362644769754,-2.38522561970891,
3.81637226963152));
#28312=CARTESIAN_POINT('Ctrl Pts',(-28.8469549569745,-2.30566301000398,
3.86618542447976));
#28313=CARTESIAN_POINT('Ctrl Pts',(-28.3649107668198,-2.15388373878846,
3.95147475669815));
#28314=CARTESIAN_POINT('Ctrl Pts',(-28.2228041159262,-2.09926959675711,
3.98096555586596));
#28315=CARTESIAN_POINT('Ctrl Pts',(-28.0241068899402,-2.0044965746748,4.02905055581734));
#28316=CARTESIAN_POINT('Ctrl Pts',(-27.9636909773592,-1.97231644998907,
4.04490878055012));
#28317=CARTESIAN_POINT('Ctrl Pts',(-27.8544921443592,-1.90676795709293,
4.07621824485302));
#28318=CARTESIAN_POINT('Ctrl Pts',(-27.8074894795624,-1.87480693010739,
4.09103914533469));
#28319=CARTESIAN_POINT('Ctrl Pts',(-27.717996119642,-1.80405959074722,4.12272619838771));
#28320=CARTESIAN_POINT('Ctrl Pts',(-27.678854738298,-1.76688965222934,4.13877771020656));
#28321=CARTESIAN_POINT('Ctrl Pts',(-27.6345827386579,-1.71546336982027,
4.16023201531108));
#28322=CARTESIAN_POINT('Ctrl Pts',(-27.6209916578288,-1.69762771350756,
4.1675483668759));
#28323=CARTESIAN_POINT('Ctrl Pts',(-27.6023544151614,-1.66982067175446,
4.17873171370946));
#28324=CARTESIAN_POINT('Ctrl Pts',(-27.596433564035,-1.66037606322677,4.18249426682801));
#28325=CARTESIAN_POINT('Ctrl Pts',(-27.5851749879742,-1.64113344454058,
4.19008209711886));
#28326=CARTESIAN_POINT('Ctrl Pts',(-27.579029173103,-1.629737911742,4.19452440771899));
#28327=CARTESIAN_POINT('Ctrl Pts',(-27.566314957399,-1.60460303135711,4.20423260339357));
#28328=CARTESIAN_POINT('Ctrl Pts',(-27.5583409045667,-1.58667844241493,
4.21104108768807));
#28329=CARTESIAN_POINT('Ctrl Pts',(-27.5471329617739,-1.55801707841301,
4.22169239332151));
#28330=CARTESIAN_POINT('Ctrl Pts',(-27.5435225035856,-1.54816752802356,
4.22531583330063));
#28331=CARTESIAN_POINT('Ctrl Pts',(-27.538295100417,-1.53294663230486,4.23085142364951));
#28332=CARTESIAN_POINT('Ctrl Pts',(-27.5365840133798,-1.5277985713604,4.23271335300807));
#28333=CARTESIAN_POINT('Ctrl Pts',(-27.5332246006767,-1.51735309651292,
4.23646909393735));
#28334=CARTESIAN_POINT('Ctrl Pts',(-27.5309269955758,-1.50989843558458,
4.2391294337564));
#28335=CARTESIAN_POINT('Ctrl Pts',(-27.521793616354,-1.47955255699408,4.24991214568788));
#28336=CARTESIAN_POINT('Ctrl Pts',(-27.5111302649714,-1.43780244931942,
4.26452955000402));
#28337=CARTESIAN_POINT('Ctrl Pts',(-27.497968043987,-1.38101342313609,4.28285042068849));
#28338=CARTESIAN_POINT('',(-27.5,-2.47065947129021,7.60893171062298));
#28339=CARTESIAN_POINT('Origin',(-27.5,0.,0.));
#28340=CARTESIAN_POINT('Origin',(-43.8559375004336,0.149957969249583,-4.29423438922274));
#28341=CARTESIAN_POINT('',(-43.9253906252168,0.1469591965737,-4.20836077533825));
#28342=CARTESIAN_POINT('',(-43.7864843756504,0.1469591965737,-4.20836077533825));
#28343=CARTESIAN_POINT('Origin',(-43.8559375004335,-3.93782229046735E-15,
8.32667268468867E-14));
#28344=CARTESIAN_POINT('Ctrl Pts',(-36.4145312504336,-0.149957969249583,
4.29423438922274));
#28345=CARTESIAN_POINT('Ctrl Pts',(-36.3880729171003,-2.62923534983068,
4.20765611530936));
#28346=CARTESIAN_POINT('Ctrl Pts',(-36.3616145837669,-3.79389505549643,
2.01724978374131));
#28347=CARTESIAN_POINT('Ctrl Pts',(-36.3351562504336,-4.95855476116219,
-0.173156547826752));
#28348=CARTESIAN_POINT('Ctrl Pts',(-36.3086979171003,-3.64393708624685,
-2.27698460548143));
#28349=CARTESIAN_POINT('Ctrl Pts',(-36.2822395837669,-2.32931941133151,
-4.38081266313611));
#28350=CARTESIAN_POINT('Ctrl Pts',(-36.2557812504336,0.149957969249583,
-4.29423438922274));
#28351=CARTESIAN_POINT('Ctrl Pts',(-36.2293229171003,2.62923534983068,-4.20765611530936));
#28352=CARTESIAN_POINT('Ctrl Pts',(-36.2028645837669,3.79389505549643,-2.0172497837413));
#28353=CARTESIAN_POINT('Ctrl Pts',(-36.1764062504336,4.95855476116219,0.173156547826753));
#28354=CARTESIAN_POINT('Ctrl Pts',(-36.1499479171003,3.64393708624685,2.27698460548143));
#28355=CARTESIAN_POINT('Ctrl Pts',(-36.1234895837669,2.32931941133151,4.38081266313611));
#28356=CARTESIAN_POINT('Ctrl Pts',(-36.0970312504336,-0.149957969249583,
4.29423438922274));
#28357=CARTESIAN_POINT('Ctrl Pts',(-36.3748437504336,-0.149957969249583,
4.29423438922274));
#28358=CARTESIAN_POINT('Ctrl Pts',(-36.3483854171003,-2.62923534983068,
4.20765611530936));
#28359=CARTESIAN_POINT('Ctrl Pts',(-36.3219270837669,-3.79389505549643,
2.01724978374131));
#28360=CARTESIAN_POINT('Ctrl Pts',(-36.2954687504336,-4.95855476116219,
-0.173156547826752));
#28361=CARTESIAN_POINT('Ctrl Pts',(-36.2690104171003,-3.64393708624685,
-2.27698460548143));
#28362=CARTESIAN_POINT('Ctrl Pts',(-36.2425520837669,-2.32931941133151,
-4.38081266313611));
#28363=CARTESIAN_POINT('Ctrl Pts',(-36.2160937504336,0.149957969249583,
-4.29423438922274));
#28364=CARTESIAN_POINT('Ctrl Pts',(-36.1896354171003,2.62923534983068,-4.20765611530936));
#28365=CARTESIAN_POINT('Ctrl Pts',(-36.1631770837669,3.79389505549644,-2.0172497837413));
#28366=CARTESIAN_POINT('Ctrl Pts',(-36.1367187504336,4.95855476116219,0.173156547826753));
#28367=CARTESIAN_POINT('Ctrl Pts',(-36.1102604171003,3.64393708624685,2.27698460548143));
#28368=CARTESIAN_POINT('Ctrl Pts',(-36.0838020837669,2.32931941133151,4.38081266313611));
#28369=CARTESIAN_POINT('Ctrl Pts',(-36.0573437504336,-0.149957969249583,
4.29423438922274));
#28370=CARTESIAN_POINT('Ctrl Pts',(-43.975,0.143960423897816,-4.12248716145376));
#28371=CARTESIAN_POINT('Ctrl Pts',(-43.9485416666667,2.52407949629392,-4.03937157196371));
#28372=CARTESIAN_POINT('Ctrl Pts',(-43.9220833333334,3.64215882054307,-1.9365701964918));
#28373=CARTESIAN_POINT('Ctrl Pts',(-43.895625,4.76023814479221,0.166231178980113));
#28374=CARTESIAN_POINT('Ctrl Pts',(-43.8691666666667,3.49819839664525,2.18591696496197));
#28375=CARTESIAN_POINT('Ctrl Pts',(-43.8427083333333,2.23615864849829,4.20560275094382));
#28376=CARTESIAN_POINT('Ctrl Pts',(-43.81625,-0.143960423897816,4.12248716145376));
#28377=CARTESIAN_POINT('Ctrl Pts',(-43.7897916666667,-2.52407949629392,
4.03937157196371));
#28378=CARTESIAN_POINT('Ctrl Pts',(-43.7633333333333,-3.64215882054307,
1.9365701964918));
#28379=CARTESIAN_POINT('Ctrl Pts',(-43.736875,-4.76023814479221,-0.166231178980113));
#28380=CARTESIAN_POINT('Ctrl Pts',(-43.7104166666667,-3.49819839664525,
-2.18591696496196));
#28381=CARTESIAN_POINT('Ctrl Pts',(-43.6839583333334,-2.23615864849829,
-4.20560275094382));
#28382=CARTESIAN_POINT('Ctrl Pts',(-43.6575,0.143960423897816,-4.12248716145376));
#28383=CARTESIAN_POINT('Ctrl Pts',(-43.6310416666667,2.52407949629392,-4.03937157196371));
#28384=CARTESIAN_POINT('Ctrl Pts',(-43.6045833333334,3.64215882054307,-1.9365701964918));
#28385=CARTESIAN_POINT('Ctrl Pts',(-43.578125,4.76023814479221,0.166231178980113));
#28386=CARTESIAN_POINT('Ctrl Pts',(-43.5516666666667,3.49819839664525,2.18591696496197));
#28387=CARTESIAN_POINT('Ctrl Pts',(-43.5252083333334,2.23615864849829,4.20560275094382));
#28388=CARTESIAN_POINT('Ctrl Pts',(-43.49875,-0.143960423897816,4.12248716145376));
#28389=CARTESIAN_POINT('Ctrl Pts',(-43.4722916666667,-2.52407949629392,
4.03937157196371));
#28390=CARTESIAN_POINT('Ctrl Pts',(-43.4458333333334,-3.64215882054307,
1.9365701964918));
#28391=CARTESIAN_POINT('Ctrl Pts',(-43.419375,-4.76023814479221,-0.166231178980113));
#28392=CARTESIAN_POINT('Ctrl Pts',(-43.3929166666667,-3.49819839664525,
-2.18591696496196));
#28393=CARTESIAN_POINT('Ctrl Pts',(-43.3664583333334,-2.23615864849829,
-4.20560275094382));
#28394=CARTESIAN_POINT('Ctrl Pts',(-43.34,0.143960423897816,-4.12248716145376));
#28395=CARTESIAN_POINT('Ctrl Pts',(-43.3135416666667,2.52407949629392,-4.03937157196371));
#28396=CARTESIAN_POINT('Ctrl Pts',(-43.2870833333333,3.64215882054307,-1.9365701964918));
#28397=CARTESIAN_POINT('Ctrl Pts',(-43.260625,4.76023814479221,0.166231178980113));
#28398=CARTESIAN_POINT('Ctrl Pts',(-43.2341666666667,3.49819839664525,2.18591696496197));
#28399=CARTESIAN_POINT('Ctrl Pts',(-43.2077083333333,2.23615864849829,4.20560275094382));
#28400=CARTESIAN_POINT('Ctrl Pts',(-43.18125,-0.143960423897816,4.12248716145376));
#28401=CARTESIAN_POINT('Ctrl Pts',(-43.1547916666667,-2.52407949629392,
4.03937157196371));
#28402=CARTESIAN_POINT('Ctrl Pts',(-43.1283333333333,-3.64215882054307,
1.9365701964918));
#28403=CARTESIAN_POINT('Ctrl Pts',(-43.101875,-4.76023814479221,-0.166231178980113));
#28404=CARTESIAN_POINT('Ctrl Pts',(-43.0754166666667,-3.49819839664525,
-2.18591696496196));
#28405=CARTESIAN_POINT('Ctrl Pts',(-43.0489583333333,-2.23615864849829,
-4.20560275094382));
#28406=CARTESIAN_POINT('Ctrl Pts',(-43.0225,0.143960423897816,-4.12248716145376));
#28407=CARTESIAN_POINT('Ctrl Pts',(-42.9960416666667,2.52407949629392,-4.03937157196371));
#28408=CARTESIAN_POINT('Ctrl Pts',(-42.9695833333334,3.64215882054307,-1.9365701964918));
#28409=CARTESIAN_POINT('Ctrl Pts',(-42.943125,4.76023814479221,0.166231178980113));
#28410=CARTESIAN_POINT('Ctrl Pts',(-42.9166666666667,3.49819839664525,2.18591696496197));
#28411=CARTESIAN_POINT('Ctrl Pts',(-42.8902083333333,2.23615864849829,4.20560275094382));
#28412=CARTESIAN_POINT('Ctrl Pts',(-42.86375,-0.143960423897816,4.12248716145376));
#28413=CARTESIAN_POINT('Ctrl Pts',(-42.8372916666667,-2.52407949629392,
4.03937157196371));
#28414=CARTESIAN_POINT('Ctrl Pts',(-42.8108333333333,-3.64215882054307,
1.9365701964918));
#28415=CARTESIAN_POINT('Ctrl Pts',(-42.784375,-4.76023814479221,-0.166231178980113));
#28416=CARTESIAN_POINT('Ctrl Pts',(-42.7579166666667,-3.49819839664525,
-2.18591696496196));
#28417=CARTESIAN_POINT('Ctrl Pts',(-42.7314583333334,-2.23615864849829,
-4.20560275094382));
#28418=CARTESIAN_POINT('Ctrl Pts',(-42.705,0.143960423897816,-4.12248716145376));
#28419=CARTESIAN_POINT('Ctrl Pts',(-42.6785416666667,2.52407949629392,-4.03937157196371));
#28420=CARTESIAN_POINT('Ctrl Pts',(-42.6520833333333,3.64215882054307,-1.9365701964918));
#28421=CARTESIAN_POINT('Ctrl Pts',(-42.625625,4.76023814479221,0.166231178980113));
#28422=CARTESIAN_POINT('Ctrl Pts',(-42.5991666666667,3.49819839664525,2.18591696496197));
#28423=CARTESIAN_POINT('Ctrl Pts',(-42.5727083333334,2.23615864849829,4.20560275094382));
#28424=CARTESIAN_POINT('Ctrl Pts',(-42.54625,-0.143960423897816,4.12248716145376));
#28425=CARTESIAN_POINT('Ctrl Pts',(-42.5197916666667,-2.52407949629392,
4.03937157196371));
#28426=CARTESIAN_POINT('Ctrl Pts',(-42.4933333333334,-3.64215882054307,
1.9365701964918));
#28427=CARTESIAN_POINT('Ctrl Pts',(-42.466875,-4.76023814479221,-0.166231178980113));
#28428=CARTESIAN_POINT('Ctrl Pts',(-42.4404166666667,-3.49819839664525,
-2.18591696496196));
#28429=CARTESIAN_POINT('Ctrl Pts',(-42.4139583333333,-2.23615864849829,
-4.20560275094382));
#28430=CARTESIAN_POINT('Ctrl Pts',(-42.3875,0.143960423897816,-4.12248716145376));
#28431=CARTESIAN_POINT('Ctrl Pts',(-42.3610416666667,2.52407949629392,-4.03937157196371));
#28432=CARTESIAN_POINT('Ctrl Pts',(-42.3345833333333,3.64215882054307,-1.9365701964918));
#28433=CARTESIAN_POINT('Ctrl Pts',(-42.308125,4.76023814479221,0.166231178980113));
#28434=CARTESIAN_POINT('Ctrl Pts',(-42.2816666666667,3.49819839664525,2.18591696496197));
#28435=CARTESIAN_POINT('Ctrl Pts',(-42.2552083333333,2.23615864849829,4.20560275094382));
#28436=CARTESIAN_POINT('Ctrl Pts',(-42.22875,-0.143960423897816,4.12248716145376));
#28437=CARTESIAN_POINT('Ctrl Pts',(-42.2022916666667,-2.52407949629392,
4.03937157196371));
#28438=CARTESIAN_POINT('Ctrl Pts',(-42.1758333333334,-3.64215882054307,
1.9365701964918));
#28439=CARTESIAN_POINT('Ctrl Pts',(-42.149375,-4.76023814479221,-0.166231178980113));
#28440=CARTESIAN_POINT('Ctrl Pts',(-42.1229166666667,-3.49819839664525,
-2.18591696496196));
#28441=CARTESIAN_POINT('Ctrl Pts',(-42.0964583333333,-2.23615864849829,
-4.20560275094382));
#28442=CARTESIAN_POINT('Ctrl Pts',(-42.07,0.143960423897816,-4.12248716145376));
#28443=CARTESIAN_POINT('Ctrl Pts',(-42.0435416666667,2.52407949629392,-4.03937157196371));
#28444=CARTESIAN_POINT('Ctrl Pts',(-42.0170833333334,3.64215882054307,-1.9365701964918));
#28445=CARTESIAN_POINT('Ctrl Pts',(-41.990625,4.76023814479221,0.166231178980113));
#28446=CARTESIAN_POINT('Ctrl Pts',(-41.9641666666667,3.49819839664525,2.18591696496197));
#28447=CARTESIAN_POINT('Ctrl Pts',(-41.9377083333333,2.23615864849829,4.20560275094382));
#28448=CARTESIAN_POINT('Ctrl Pts',(-41.91125,-0.143960423897816,4.12248716145376));
#28449=CARTESIAN_POINT('Ctrl Pts',(-41.8847916666667,-2.52407949629392,
4.03937157196371));
#28450=CARTESIAN_POINT('Ctrl Pts',(-41.8583333333333,-3.64215882054307,
1.9365701964918));
#28451=CARTESIAN_POINT('Ctrl Pts',(-41.831875,-4.76023814479221,-0.166231178980113));
#28452=CARTESIAN_POINT('Ctrl Pts',(-41.8054166666667,-3.49819839664525,
-2.18591696496196));
#28453=CARTESIAN_POINT('Ctrl Pts',(-41.7789583333333,-2.23615864849829,
-4.20560275094382));
#28454=CARTESIAN_POINT('Ctrl Pts',(-41.7525,0.143960423897816,-4.12248716145376));
#28455=CARTESIAN_POINT('Ctrl Pts',(-41.7260416666667,2.52407949629392,-4.03937157196371));
#28456=CARTESIAN_POINT('Ctrl Pts',(-41.6995833333333,3.64215882054307,-1.9365701964918));
#28457=CARTESIAN_POINT('Ctrl Pts',(-41.673125,4.76023814479221,0.166231178980113));
#28458=CARTESIAN_POINT('Ctrl Pts',(-41.6466666666667,3.49819839664525,2.18591696496197));
#28459=CARTESIAN_POINT('Ctrl Pts',(-41.6202083333334,2.23615864849829,4.20560275094382));
#28460=CARTESIAN_POINT('Ctrl Pts',(-41.59375,-0.143960423897816,4.12248716145376));
#28461=CARTESIAN_POINT('Ctrl Pts',(-41.5672916666667,-2.52407949629392,
4.03937157196371));
#28462=CARTESIAN_POINT('Ctrl Pts',(-41.5408333333334,-3.64215882054307,
1.9365701964918));
#28463=CARTESIAN_POINT('Ctrl Pts',(-41.514375,-4.76023814479221,-0.166231178980113));
#28464=CARTESIAN_POINT('Ctrl Pts',(-41.4879166666667,-3.49819839664525,
-2.18591696496196));
#28465=CARTESIAN_POINT('Ctrl Pts',(-41.4614583333333,-2.23615864849829,
-4.20560275094382));
#28466=CARTESIAN_POINT('Ctrl Pts',(-41.435,0.143960423897816,-4.12248716145376));
#28467=CARTESIAN_POINT('Ctrl Pts',(-41.4085416666667,2.52407949629392,-4.03937157196371));
#28468=CARTESIAN_POINT('Ctrl Pts',(-41.3820833333333,3.64215882054307,-1.9365701964918));
#28469=CARTESIAN_POINT('Ctrl Pts',(-41.355625,4.76023814479221,0.166231178980113));
#28470=CARTESIAN_POINT('Ctrl Pts',(-41.3291666666667,3.49819839664525,2.18591696496197));
#28471=CARTESIAN_POINT('Ctrl Pts',(-41.3027083333333,2.23615864849829,4.20560275094382));
#28472=CARTESIAN_POINT('Ctrl Pts',(-41.27625,-0.143960423897816,4.12248716145376));
#28473=CARTESIAN_POINT('Ctrl Pts',(-41.2497916666667,-2.52407949629392,
4.03937157196371));
#28474=CARTESIAN_POINT('Ctrl Pts',(-41.2233333333334,-3.64215882054307,
1.9365701964918));
#28475=CARTESIAN_POINT('Ctrl Pts',(-41.196875,-4.76023814479221,-0.166231178980113));
#28476=CARTESIAN_POINT('Ctrl Pts',(-41.1704166666667,-3.49819839664525,
-2.18591696496196));
#28477=CARTESIAN_POINT('Ctrl Pts',(-41.1439583333334,-2.23615864849829,
-4.20560275094382));
#28478=CARTESIAN_POINT('Ctrl Pts',(-41.1175,0.143960423897816,-4.12248716145376));
#28479=CARTESIAN_POINT('Ctrl Pts',(-41.0910416666667,2.52407949629392,-4.03937157196371));
#28480=CARTESIAN_POINT('Ctrl Pts',(-41.0645833333334,3.64215882054307,-1.9365701964918));
#28481=CARTESIAN_POINT('Ctrl Pts',(-41.038125,4.76023814479221,0.166231178980113));
#28482=CARTESIAN_POINT('Ctrl Pts',(-41.0116666666667,3.49819839664525,2.18591696496197));
#28483=CARTESIAN_POINT('Ctrl Pts',(-40.9852083333334,2.23615864849829,4.20560275094382));
#28484=CARTESIAN_POINT('Ctrl Pts',(-40.95875,-0.143960423897816,4.12248716145376));
#28485=CARTESIAN_POINT('Ctrl Pts',(-40.9322916666667,-2.52407949629392,
4.03937157196371));
#28486=CARTESIAN_POINT('Ctrl Pts',(-40.9058333333333,-3.64215882054307,
1.9365701964918));
#28487=CARTESIAN_POINT('Ctrl Pts',(-40.879375,-4.76023814479221,-0.166231178980113));
#28488=CARTESIAN_POINT('Ctrl Pts',(-40.8529166666667,-3.49819839664525,
-2.18591696496196));
#28489=CARTESIAN_POINT('Ctrl Pts',(-40.8264583333333,-2.23615864849829,
-4.20560275094382));
#28490=CARTESIAN_POINT('Ctrl Pts',(-40.8,0.143960423897816,-4.12248716145376));
#28491=CARTESIAN_POINT('Ctrl Pts',(-40.7735416666667,2.52407949629392,-4.03937157196371));
#28492=CARTESIAN_POINT('Ctrl Pts',(-40.7470833333333,3.64215882054307,-1.9365701964918));
#28493=CARTESIAN_POINT('Ctrl Pts',(-40.720625,4.76023814479221,0.166231178980113));
#28494=CARTESIAN_POINT('Ctrl Pts',(-40.6941666666667,3.49819839664525,2.18591696496197));
#28495=CARTESIAN_POINT('Ctrl Pts',(-40.6677083333334,2.23615864849829,4.20560275094382));
#28496=CARTESIAN_POINT('Ctrl Pts',(-40.64125,-0.143960423897816,4.12248716145376));
#28497=CARTESIAN_POINT('Ctrl Pts',(-40.6147916666667,-2.52407949629392,
4.03937157196371));
#28498=CARTESIAN_POINT('Ctrl Pts',(-40.5883333333334,-3.64215882054307,
1.9365701964918));
#28499=CARTESIAN_POINT('Ctrl Pts',(-40.561875,-4.76023814479221,-0.166231178980113));
#28500=CARTESIAN_POINT('Ctrl Pts',(-40.5354166666667,-3.49819839664525,
-2.18591696496196));
#28501=CARTESIAN_POINT('Ctrl Pts',(-40.5089583333333,-2.23615864849829,
-4.20560275094382));
#28502=CARTESIAN_POINT('Ctrl Pts',(-40.4825,0.143960423897816,-4.12248716145376));
#28503=CARTESIAN_POINT('Ctrl Pts',(-40.4560416666667,2.52407949629392,-4.03937157196371));
#28504=CARTESIAN_POINT('Ctrl Pts',(-40.4295833333333,3.64215882054307,-1.9365701964918));
#28505=CARTESIAN_POINT('Ctrl Pts',(-40.403125,4.76023814479221,0.166231178980113));
#28506=CARTESIAN_POINT('Ctrl Pts',(-40.3766666666667,3.49819839664525,2.18591696496197));
#28507=CARTESIAN_POINT('Ctrl Pts',(-40.3502083333333,2.23615864849829,4.20560275094382));
#28508=CARTESIAN_POINT('Ctrl Pts',(-40.32375,-0.143960423897816,4.12248716145376));
#28509=CARTESIAN_POINT('Ctrl Pts',(-40.2972916666667,-2.52407949629392,
4.03937157196371));
#28510=CARTESIAN_POINT('Ctrl Pts',(-40.2708333333333,-3.64215882054307,
1.9365701964918));
#28511=CARTESIAN_POINT('Ctrl Pts',(-40.244375,-4.76023814479221,-0.166231178980113));
#28512=CARTESIAN_POINT('Ctrl Pts',(-40.2179166666667,-3.49819839664525,
-2.18591696496196));
#28513=CARTESIAN_POINT('Ctrl Pts',(-40.1914583333333,-2.23615864849829,
-4.20560275094382));
#28514=CARTESIAN_POINT('Ctrl Pts',(-40.165,0.143960423897816,-4.12248716145376));
#28515=CARTESIAN_POINT('Ctrl Pts',(-40.1385416666667,2.52407949629392,-4.03937157196371));
#28516=CARTESIAN_POINT('Ctrl Pts',(-40.1120833333334,3.64215882054307,-1.9365701964918));
#28517=CARTESIAN_POINT('Ctrl Pts',(-40.085625,4.76023814479221,0.166231178980113));
#28518=CARTESIAN_POINT('Ctrl Pts',(-40.0591666666667,3.49819839664525,2.18591696496197));
#28519=CARTESIAN_POINT('Ctrl Pts',(-40.0327083333333,2.23615864849829,4.20560275094382));
#28520=CARTESIAN_POINT('Ctrl Pts',(-40.00625,-0.143960423897816,4.12248716145376));
#28521=CARTESIAN_POINT('Ctrl Pts',(-39.9797916666667,-2.52407949629392,
4.03937157196371));
#28522=CARTESIAN_POINT('Ctrl Pts',(-39.9533333333333,-3.64215882054307,
1.9365701964918));
#28523=CARTESIAN_POINT('Ctrl Pts',(-39.926875,-4.76023814479221,-0.166231178980113));
#28524=CARTESIAN_POINT('Ctrl Pts',(-39.9004166666667,-3.49819839664525,
-2.18591696496196));
#28525=CARTESIAN_POINT('Ctrl Pts',(-39.8739583333333,-2.23615864849829,
-4.20560275094382));
#28526=CARTESIAN_POINT('Ctrl Pts',(-39.8475,0.143960423897816,-4.12248716145376));
#28527=CARTESIAN_POINT('Ctrl Pts',(-39.8210416666667,2.52407949629392,-4.03937157196371));
#28528=CARTESIAN_POINT('Ctrl Pts',(-39.7945833333333,3.64215882054307,-1.9365701964918));
#28529=CARTESIAN_POINT('Ctrl Pts',(-39.768125,4.76023814479221,0.166231178980113));
#28530=CARTESIAN_POINT('Ctrl Pts',(-39.7416666666667,3.49819839664525,2.18591696496197));
#28531=CARTESIAN_POINT('Ctrl Pts',(-39.7152083333334,2.23615864849829,4.20560275094382));
#28532=CARTESIAN_POINT('Ctrl Pts',(-39.68875,-0.143960423897816,4.12248716145376));
#28533=CARTESIAN_POINT('Ctrl Pts',(-39.6622916666667,-2.52407949629392,
4.03937157196371));
#28534=CARTESIAN_POINT('Ctrl Pts',(-39.6358333333333,-3.64215882054307,
1.9365701964918));
#28535=CARTESIAN_POINT('Ctrl Pts',(-39.609375,-4.76023814479221,-0.166231178980113));
#28536=CARTESIAN_POINT('Ctrl Pts',(-39.5829166666667,-3.49819839664525,
-2.18591696496196));
#28537=CARTESIAN_POINT('Ctrl Pts',(-39.5564583333333,-2.23615864849829,
-4.20560275094382));
#28538=CARTESIAN_POINT('Ctrl Pts',(-39.53,0.143960423897816,-4.12248716145376));
#28539=CARTESIAN_POINT('Ctrl Pts',(-39.5035416666667,2.52407949629392,-4.03937157196371));
#28540=CARTESIAN_POINT('Ctrl Pts',(-39.4770833333333,3.64215882054307,-1.9365701964918));
#28541=CARTESIAN_POINT('Ctrl Pts',(-39.450625,4.76023814479221,0.166231178980113));
#28542=CARTESIAN_POINT('Ctrl Pts',(-39.4241666666667,3.49819839664525,2.18591696496197));
#28543=CARTESIAN_POINT('Ctrl Pts',(-39.3977083333333,2.23615864849829,4.20560275094382));
#28544=CARTESIAN_POINT('Ctrl Pts',(-39.37125,-0.143960423897816,4.12248716145376));
#28545=CARTESIAN_POINT('Ctrl Pts',(-39.3447916666667,-2.52407949629392,
4.03937157196371));
#28546=CARTESIAN_POINT('Ctrl Pts',(-39.3183333333333,-3.64215882054307,
1.9365701964918));
#28547=CARTESIAN_POINT('Ctrl Pts',(-39.291875,-4.76023814479221,-0.166231178980113));
#28548=CARTESIAN_POINT('Ctrl Pts',(-39.2654166666667,-3.49819839664525,
-2.18591696496196));
#28549=CARTESIAN_POINT('Ctrl Pts',(-39.2389583333333,-2.23615864849829,
-4.20560275094382));
#28550=CARTESIAN_POINT('Ctrl Pts',(-39.2125,0.143960423897816,-4.12248716145376));
#28551=CARTESIAN_POINT('Ctrl Pts',(-39.1860416666667,2.52407949629392,-4.03937157196371));
#28552=CARTESIAN_POINT('Ctrl Pts',(-39.1595833333333,3.64215882054307,-1.9365701964918));
#28553=CARTESIAN_POINT('Ctrl Pts',(-39.133125,4.76023814479221,0.166231178980113));
#28554=CARTESIAN_POINT('Ctrl Pts',(-39.1066666666667,3.49819839664525,2.18591696496197));
#28555=CARTESIAN_POINT('Ctrl Pts',(-39.0802083333333,2.23615864849829,4.20560275094382));
#28556=CARTESIAN_POINT('Ctrl Pts',(-39.05375,-0.143960423897816,4.12248716145376));
#28557=CARTESIAN_POINT('Ctrl Pts',(-39.0272916666667,-2.52407949629392,
4.03937157196371));
#28558=CARTESIAN_POINT('Ctrl Pts',(-39.0008333333333,-3.64215882054307,
1.9365701964918));
#28559=CARTESIAN_POINT('Ctrl Pts',(-38.974375,-4.76023814479221,-0.166231178980113));
#28560=CARTESIAN_POINT('Ctrl Pts',(-38.9479166666667,-3.49819839664525,
-2.18591696496196));
#28561=CARTESIAN_POINT('Ctrl Pts',(-38.9214583333333,-2.23615864849829,
-4.20560275094382));
#28562=CARTESIAN_POINT('Ctrl Pts',(-38.895,0.143960423897816,-4.12248716145376));
#28563=CARTESIAN_POINT('Ctrl Pts',(-38.8685416666667,2.52407949629392,-4.03937157196371));
#28564=CARTESIAN_POINT('Ctrl Pts',(-38.8420833333333,3.64215882054307,-1.9365701964918));
#28565=CARTESIAN_POINT('Ctrl Pts',(-38.815625,4.76023814479221,0.166231178980113));
#28566=CARTESIAN_POINT('Ctrl Pts',(-38.7891666666667,3.49819839664525,2.18591696496197));
#28567=CARTESIAN_POINT('Ctrl Pts',(-38.7627083333334,2.23615864849829,4.20560275094382));
#28568=CARTESIAN_POINT('Ctrl Pts',(-38.73625,-0.143960423897816,4.12248716145376));
#28569=CARTESIAN_POINT('Ctrl Pts',(-38.7097916666667,-2.52407949629392,
4.03937157196371));
#28570=CARTESIAN_POINT('Ctrl Pts',(-38.6833333333333,-3.64215882054307,
1.9365701964918));
#28571=CARTESIAN_POINT('Ctrl Pts',(-38.656875,-4.76023814479221,-0.166231178980113));
#28572=CARTESIAN_POINT('Ctrl Pts',(-38.6304166666667,-3.49819839664525,
-2.18591696496196));
#28573=CARTESIAN_POINT('Ctrl Pts',(-38.6039583333333,-2.23615864849829,
-4.20560275094382));
#28574=CARTESIAN_POINT('Ctrl Pts',(-38.5775,0.143960423897816,-4.12248716145376));
#28575=CARTESIAN_POINT('Ctrl Pts',(-38.5510416666667,2.52407949629392,-4.03937157196371));
#28576=CARTESIAN_POINT('Ctrl Pts',(-38.5245833333333,3.64215882054307,-1.9365701964918));
#28577=CARTESIAN_POINT('Ctrl Pts',(-38.498125,4.76023814479221,0.166231178980113));
#28578=CARTESIAN_POINT('Ctrl Pts',(-38.4716666666667,3.49819839664525,2.18591696496197));
#28579=CARTESIAN_POINT('Ctrl Pts',(-38.4452083333333,2.23615864849829,4.20560275094382));
#28580=CARTESIAN_POINT('Ctrl Pts',(-38.41875,-0.143960423897816,4.12248716145376));
#28581=CARTESIAN_POINT('Ctrl Pts',(-38.3922916666667,-2.52407949629392,
4.03937157196371));
#28582=CARTESIAN_POINT('Ctrl Pts',(-38.3658333333334,-3.64215882054307,
1.9365701964918));
#28583=CARTESIAN_POINT('Ctrl Pts',(-38.339375,-4.76023814479221,-0.166231178980113));
#28584=CARTESIAN_POINT('Ctrl Pts',(-38.3129166666667,-3.49819839664525,
-2.18591696496196));
#28585=CARTESIAN_POINT('Ctrl Pts',(-38.2864583333333,-2.23615864849829,
-4.20560275094382));
#28586=CARTESIAN_POINT('Ctrl Pts',(-38.26,0.143960423897816,-4.12248716145376));
#28587=CARTESIAN_POINT('Ctrl Pts',(-38.2335416666667,2.52407949629392,-4.03937157196371));
#28588=CARTESIAN_POINT('Ctrl Pts',(-38.2070833333333,3.64215882054307,-1.9365701964918));
#28589=CARTESIAN_POINT('Ctrl Pts',(-38.180625,4.76023814479221,0.166231178980113));
#28590=CARTESIAN_POINT('Ctrl Pts',(-38.1541666666667,3.49819839664525,2.18591696496197));
#28591=CARTESIAN_POINT('Ctrl Pts',(-38.1277083333333,2.23615864849829,4.20560275094382));
#28592=CARTESIAN_POINT('Ctrl Pts',(-38.10125,-0.143960423897816,4.12248716145376));
#28593=CARTESIAN_POINT('Ctrl Pts',(-38.0747916666667,-2.52407949629392,
4.03937157196371));
#28594=CARTESIAN_POINT('Ctrl Pts',(-38.0483333333333,-3.64215882054307,
1.9365701964918));
#28595=CARTESIAN_POINT('Ctrl Pts',(-38.021875,-4.76023814479221,-0.166231178980113));
#28596=CARTESIAN_POINT('Ctrl Pts',(-37.9954166666667,-3.49819839664525,
-2.18591696496196));
#28597=CARTESIAN_POINT('Ctrl Pts',(-37.9689583333333,-2.23615864849829,
-4.20560275094382));
#28598=CARTESIAN_POINT('Ctrl Pts',(-37.9425,0.143960423897816,-4.12248716145376));
#28599=CARTESIAN_POINT('Ctrl Pts',(-37.9160416666667,2.52407949629392,-4.03937157196371));
#28600=CARTESIAN_POINT('Ctrl Pts',(-37.8895833333333,3.64215882054307,-1.9365701964918));
#28601=CARTESIAN_POINT('Ctrl Pts',(-37.863125,4.76023814479221,0.166231178980113));
#28602=CARTESIAN_POINT('Ctrl Pts',(-37.8366666666667,3.49819839664525,2.18591696496197));
#28603=CARTESIAN_POINT('Ctrl Pts',(-37.8102083333333,2.23615864849829,4.20560275094382));
#28604=CARTESIAN_POINT('Ctrl Pts',(-37.78375,-0.143960423897816,4.12248716145376));
#28605=CARTESIAN_POINT('Ctrl Pts',(-37.7572916666667,-2.52407949629392,
4.03937157196371));
#28606=CARTESIAN_POINT('Ctrl Pts',(-37.7308333333333,-3.64215882054307,
1.9365701964918));
#28607=CARTESIAN_POINT('Ctrl Pts',(-37.704375,-4.76023814479221,-0.166231178980113));
#28608=CARTESIAN_POINT('Ctrl Pts',(-37.6779166666667,-3.49819839664525,
-2.18591696496196));
#28609=CARTESIAN_POINT('Ctrl Pts',(-37.6514583333333,-2.23615864849829,
-4.20560275094382));
#28610=CARTESIAN_POINT('Ctrl Pts',(-37.625,0.143960423897816,-4.12248716145376));
#28611=CARTESIAN_POINT('Ctrl Pts',(-37.5985416666667,2.52407949629392,-4.03937157196371));
#28612=CARTESIAN_POINT('Ctrl Pts',(-37.5720833333333,3.64215882054307,-1.9365701964918));
#28613=CARTESIAN_POINT('Ctrl Pts',(-37.545625,4.76023814479221,0.166231178980113));
#28614=CARTESIAN_POINT('Ctrl Pts',(-37.5191666666667,3.49819839664525,2.18591696496197));
#28615=CARTESIAN_POINT('Ctrl Pts',(-37.4927083333333,2.23615864849829,4.20560275094382));
#28616=CARTESIAN_POINT('Ctrl Pts',(-37.46625,-0.143960423897816,4.12248716145376));
#28617=CARTESIAN_POINT('Ctrl Pts',(-37.4397916666667,-2.52407949629392,
4.03937157196371));
#28618=CARTESIAN_POINT('Ctrl Pts',(-37.4133333333334,-3.64215882054307,
1.9365701964918));
#28619=CARTESIAN_POINT('Ctrl Pts',(-37.386875,-4.76023814479221,-0.166231178980113));
#28620=CARTESIAN_POINT('Ctrl Pts',(-37.3604166666667,-3.49819839664525,
-2.18591696496196));
#28621=CARTESIAN_POINT('Ctrl Pts',(-37.3339583333333,-2.23615864849829,
-4.20560275094382));
#28622=CARTESIAN_POINT('Ctrl Pts',(-37.3075,0.143960423897816,-4.12248716145376));
#28623=CARTESIAN_POINT('Ctrl Pts',(-37.2810416666667,2.52407949629392,-4.03937157196371));
#28624=CARTESIAN_POINT('Ctrl Pts',(-37.2545833333334,3.64215882054307,-1.9365701964918));
#28625=CARTESIAN_POINT('Ctrl Pts',(-37.228125,4.76023814479221,0.166231178980113));
#28626=CARTESIAN_POINT('Ctrl Pts',(-37.2016666666667,3.49819839664525,2.18591696496197));
#28627=CARTESIAN_POINT('Ctrl Pts',(-37.1752083333334,2.23615864849829,4.20560275094382));
#28628=CARTESIAN_POINT('Ctrl Pts',(-37.14875,-0.143960423897816,4.12248716145376));
#28629=CARTESIAN_POINT('Ctrl Pts',(-37.1222916666667,-2.52407949629392,
4.03937157196371));
#28630=CARTESIAN_POINT('Ctrl Pts',(-37.0958333333333,-3.64215882054307,
1.9365701964918));
#28631=CARTESIAN_POINT('Ctrl Pts',(-37.069375,-4.76023814479221,-0.166231178980113));
#28632=CARTESIAN_POINT('Ctrl Pts',(-37.0429166666667,-3.49819839664525,
-2.18591696496196));
#28633=CARTESIAN_POINT('Ctrl Pts',(-37.0164583333333,-2.23615864849829,
-4.20560275094382));
#28634=CARTESIAN_POINT('Ctrl Pts',(-36.99,0.143960423897816,-4.12248716145376));
#28635=CARTESIAN_POINT('Ctrl Pts',(-36.9635416666667,2.52407949629392,-4.03937157196371));
#28636=CARTESIAN_POINT('Ctrl Pts',(-36.9370833333333,3.64215882054307,-1.9365701964918));
#28637=CARTESIAN_POINT('Ctrl Pts',(-36.910625,4.76023814479221,0.166231178980113));
#28638=CARTESIAN_POINT('Ctrl Pts',(-36.8841666666667,3.49819839664525,2.18591696496197));
#28639=CARTESIAN_POINT('Ctrl Pts',(-36.8577083333333,2.23615864849829,4.20560275094382));
#28640=CARTESIAN_POINT('Ctrl Pts',(-36.83125,-0.143960423897816,4.12248716145376));
#28641=CARTESIAN_POINT('Ctrl Pts',(-36.8047916666667,-2.52407949629392,
4.03937157196371));
#28642=CARTESIAN_POINT('Ctrl Pts',(-36.7783333333333,-3.64215882054307,
1.9365701964918));
#28643=CARTESIAN_POINT('Ctrl Pts',(-36.751875,-4.76023814479221,-0.166231178980113));
#28644=CARTESIAN_POINT('Ctrl Pts',(-36.7254166666667,-3.49819839664525,
-2.18591696496196));
#28645=CARTESIAN_POINT('Ctrl Pts',(-36.6989583333333,-2.23615864849829,
-4.20560275094382));
#28646=CARTESIAN_POINT('Ctrl Pts',(-36.6725,0.143960423897816,-4.12248716145376));
#28647=CARTESIAN_POINT('Ctrl Pts',(-36.6460416666667,2.52407949629392,-4.03937157196371));
#28648=CARTESIAN_POINT('Ctrl Pts',(-36.6195833333333,3.64215882054307,-1.9365701964918));
#28649=CARTESIAN_POINT('Ctrl Pts',(-36.593125,4.76023814479221,0.166231178980113));
#28650=CARTESIAN_POINT('Ctrl Pts',(-36.5666666666667,3.49819839664525,2.18591696496197));
#28651=CARTESIAN_POINT('Ctrl Pts',(-36.5402083333333,2.23615864849829,4.20560275094382));
#28652=CARTESIAN_POINT('Ctrl Pts',(-36.51375,-0.143960423897816,4.12248716145376));
#28653=CARTESIAN_POINT('Ctrl Pts',(-36.4872916666667,-2.52407949629392,
4.03937157196371));
#28654=CARTESIAN_POINT('Ctrl Pts',(-36.4608333333334,-3.64215882054307,
1.9365701964918));
#28655=CARTESIAN_POINT('Ctrl Pts',(-36.434375,-4.76023814479221,-0.166231178980113));
#28656=CARTESIAN_POINT('Ctrl Pts',(-36.4079166666667,-3.49819839664525,
-2.18591696496196));
#28657=CARTESIAN_POINT('Ctrl Pts',(-36.3814583333333,-2.23615864849829,
-4.20560275094382));
#28658=CARTESIAN_POINT('Ctrl Pts',(-36.355,0.143960423897816,-4.12248716145376));
#28659=CARTESIAN_POINT('Ctrl Pts',(-36.3285416666667,2.52407949629392,-4.03937157196371));
#28660=CARTESIAN_POINT('Ctrl Pts',(-36.3020833333333,3.64215882054307,-1.9365701964918));
#28661=CARTESIAN_POINT('Ctrl Pts',(-36.275625,4.76023814479221,0.166231178980113));
#28662=CARTESIAN_POINT('Ctrl Pts',(-36.2491666666667,3.49819839664525,2.18591696496197));
#28663=CARTESIAN_POINT('Ctrl Pts',(-36.2227083333333,2.23615864849829,4.20560275094382));
#28664=CARTESIAN_POINT('Ctrl Pts',(-36.19625,-0.143960423897816,4.12248716145376));
#28665=CARTESIAN_POINT('Ctrl Pts',(-36.1697916666667,-2.52407949629392,
4.03937157196371));
#28666=CARTESIAN_POINT('Ctrl Pts',(-36.1433333333333,-3.64215882054307,
1.9365701964918));
#28667=CARTESIAN_POINT('Ctrl Pts',(-36.116875,-4.76023814479221,-0.166231178980113));
#28668=CARTESIAN_POINT('Ctrl Pts',(-36.0904166666667,-3.49819839664525,
-2.18591696496196));
#28669=CARTESIAN_POINT('Ctrl Pts',(-36.0639583333334,-2.23615864849829,
-4.20560275094382));
#28670=CARTESIAN_POINT('Ctrl Pts',(-36.0375,0.143960423897816,-4.12248716145376));
#28671=CARTESIAN_POINT('Ctrl Pts',(-36.0110416666667,2.52407949629392,-4.03937157196371));
#28672=CARTESIAN_POINT('Ctrl Pts',(-35.9845833333333,3.64215882054307,-1.9365701964918));
#28673=CARTESIAN_POINT('Ctrl Pts',(-35.958125,4.76023814479221,0.166231178980113));
#28674=CARTESIAN_POINT('Ctrl Pts',(-35.9316666666667,3.49819839664525,2.18591696496197));
#28675=CARTESIAN_POINT('Ctrl Pts',(-35.9052083333333,2.23615864849829,4.20560275094382));
#28676=CARTESIAN_POINT('Ctrl Pts',(-35.87875,-0.143960423897816,4.12248716145376));
#28677=CARTESIAN_POINT('Ctrl Pts',(-35.8522916666667,-2.52407949629392,
4.03937157196371));
#28678=CARTESIAN_POINT('Ctrl Pts',(-35.8258333333333,-3.64215882054307,
1.9365701964918));
#28679=CARTESIAN_POINT('Ctrl Pts',(-35.799375,-4.76023814479221,-0.166231178980113));
#28680=CARTESIAN_POINT('Ctrl Pts',(-35.7729166666667,-3.49819839664525,
-2.18591696496196));
#28681=CARTESIAN_POINT('Ctrl Pts',(-35.7464583333333,-2.23615864849829,
-4.20560275094382));
#28682=CARTESIAN_POINT('Ctrl Pts',(-35.72,0.143960423897816,-4.12248716145376));
#28683=CARTESIAN_POINT('Ctrl Pts',(-35.6935416666667,2.52407949629392,-4.03937157196371));
#28684=CARTESIAN_POINT('Ctrl Pts',(-35.6670833333334,3.64215882054307,-1.9365701964918));
#28685=CARTESIAN_POINT('Ctrl Pts',(-35.640625,4.76023814479221,0.166231178980113));
#28686=CARTESIAN_POINT('Ctrl Pts',(-35.6141666666667,3.49819839664525,2.18591696496197));
#28687=CARTESIAN_POINT('Ctrl Pts',(-35.5877083333333,2.23615864849829,4.20560275094382));
#28688=CARTESIAN_POINT('Ctrl Pts',(-35.56125,-0.143960423897816,4.12248716145376));
#28689=CARTESIAN_POINT('Ctrl Pts',(-35.5347916666667,-2.52407949629392,
4.03937157196371));
#28690=CARTESIAN_POINT('Ctrl Pts',(-35.5083333333333,-3.64215882054307,
1.9365701964918));
#28691=CARTESIAN_POINT('Ctrl Pts',(-35.481875,-4.76023814479221,-0.166231178980113));
#28692=CARTESIAN_POINT('Ctrl Pts',(-35.4554166666667,-3.49819839664525,
-2.18591696496196));
#28693=CARTESIAN_POINT('Ctrl Pts',(-35.4289583333333,-2.23615864849829,
-4.20560275094382));
#28694=CARTESIAN_POINT('Ctrl Pts',(-35.4025,0.143960423897816,-4.12248716145376));
#28695=CARTESIAN_POINT('Ctrl Pts',(-35.3760416666667,2.52407949629392,-4.03937157196371));
#28696=CARTESIAN_POINT('Ctrl Pts',(-35.3495833333333,3.64215882054307,-1.9365701964918));
#28697=CARTESIAN_POINT('Ctrl Pts',(-35.323125,4.76023814479221,0.166231178980113));
#28698=CARTESIAN_POINT('Ctrl Pts',(-35.2966666666667,3.49819839664525,2.18591696496197));
#28699=CARTESIAN_POINT('Ctrl Pts',(-35.2702083333333,2.23615864849829,4.20560275094382));
#28700=CARTESIAN_POINT('Ctrl Pts',(-35.24375,-0.143960423897816,4.12248716145376));
#28701=CARTESIAN_POINT('Ctrl Pts',(-35.2172916666667,-2.52407949629392,
4.03937157196371));
#28702=CARTESIAN_POINT('Ctrl Pts',(-35.1908333333333,-3.64215882054307,
1.9365701964918));
#28703=CARTESIAN_POINT('Ctrl Pts',(-35.164375,-4.76023814479221,-0.166231178980113));
#28704=CARTESIAN_POINT('Ctrl Pts',(-35.1379166666667,-3.49819839664525,
-2.18591696496196));
#28705=CARTESIAN_POINT('Ctrl Pts',(-35.1114583333333,-2.23615864849829,
-4.20560275094382));
#28706=CARTESIAN_POINT('Ctrl Pts',(-35.085,0.143960423897816,-4.12248716145376));
#28707=CARTESIAN_POINT('Ctrl Pts',(-35.0585416666667,2.52407949629392,-4.03937157196371));
#28708=CARTESIAN_POINT('Ctrl Pts',(-35.0320833333333,3.64215882054307,-1.9365701964918));
#28709=CARTESIAN_POINT('Ctrl Pts',(-35.005625,4.76023814479221,0.166231178980113));
#28710=CARTESIAN_POINT('Ctrl Pts',(-34.9791666666667,3.49819839664525,2.18591696496197));
#28711=CARTESIAN_POINT('Ctrl Pts',(-34.9527083333333,2.23615864849829,4.20560275094382));
#28712=CARTESIAN_POINT('Ctrl Pts',(-34.92625,-0.143960423897816,4.12248716145376));
#28713=CARTESIAN_POINT('Ctrl Pts',(-34.8997916666667,-2.52407949629392,
4.03937157196371));
#28714=CARTESIAN_POINT('Ctrl Pts',(-34.8733333333333,-3.64215882054307,
1.9365701964918));
#28715=CARTESIAN_POINT('Ctrl Pts',(-34.846875,-4.76023814479221,-0.166231178980113));
#28716=CARTESIAN_POINT('Ctrl Pts',(-34.8204166666667,-3.49819839664525,
-2.18591696496196));
#28717=CARTESIAN_POINT('Ctrl Pts',(-34.7939583333333,-2.23615864849829,
-4.20560275094382));
#28718=CARTESIAN_POINT('Ctrl Pts',(-34.7675,0.143960423897816,-4.12248716145376));
#28719=CARTESIAN_POINT('Ctrl Pts',(-34.7410416666667,2.52407949629392,-4.03937157196371));
#28720=CARTESIAN_POINT('Ctrl Pts',(-34.7145833333333,3.64215882054307,-1.9365701964918));
#28721=CARTESIAN_POINT('Ctrl Pts',(-34.688125,4.76023814479221,0.166231178980113));
#28722=CARTESIAN_POINT('Ctrl Pts',(-34.6616666666667,3.49819839664525,2.18591696496197));
#28723=CARTESIAN_POINT('Ctrl Pts',(-34.6352083333333,2.23615864849829,4.20560275094382));
#28724=CARTESIAN_POINT('Ctrl Pts',(-34.60875,-0.143960423897816,4.12248716145376));
#28725=CARTESIAN_POINT('Ctrl Pts',(-34.5822916666667,-2.52407949629392,
4.03937157196371));
#28726=CARTESIAN_POINT('Ctrl Pts',(-34.5558333333333,-3.64215882054307,
1.9365701964918));
#28727=CARTESIAN_POINT('Ctrl Pts',(-34.529375,-4.76023814479221,-0.166231178980113));
#28728=CARTESIAN_POINT('Ctrl Pts',(-34.5029166666667,-3.49819839664525,
-2.18591696496196));
#28729=CARTESIAN_POINT('Ctrl Pts',(-34.4764583333333,-2.23615864849829,
-4.20560275094382));
#28730=CARTESIAN_POINT('Ctrl Pts',(-34.45,0.143960423897816,-4.12248716145376));
#28731=CARTESIAN_POINT('Ctrl Pts',(-34.4235416666667,2.52407949629392,-4.03937157196371));
#28732=CARTESIAN_POINT('Ctrl Pts',(-34.3970833333333,3.64215882054307,-1.9365701964918));
#28733=CARTESIAN_POINT('Ctrl Pts',(-34.370625,4.76023814479221,0.166231178980113));
#28734=CARTESIAN_POINT('Ctrl Pts',(-34.3441666666667,3.49819839664525,2.18591696496197));
#28735=CARTESIAN_POINT('Ctrl Pts',(-34.3177083333333,2.23615864849829,4.20560275094382));
#28736=CARTESIAN_POINT('Ctrl Pts',(-34.29125,-0.143960423897816,4.12248716145376));
#28737=CARTESIAN_POINT('Ctrl Pts',(-34.2647916666667,-2.52407949629392,
4.03937157196371));
#28738=CARTESIAN_POINT('Ctrl Pts',(-34.2383333333333,-3.64215882054307,
1.9365701964918));
#28739=CARTESIAN_POINT('Ctrl Pts',(-34.211875,-4.76023814479221,-0.166231178980113));
#28740=CARTESIAN_POINT('Ctrl Pts',(-34.1854166666667,-3.49819839664525,
-2.18591696496196));
#28741=CARTESIAN_POINT('Ctrl Pts',(-34.1589583333333,-2.23615864849829,
-4.20560275094382));
#28742=CARTESIAN_POINT('Ctrl Pts',(-34.1325,0.143960423897816,-4.12248716145376));
#28743=CARTESIAN_POINT('Ctrl Pts',(-34.1060416666667,2.52407949629392,-4.03937157196371));
#28744=CARTESIAN_POINT('Ctrl Pts',(-34.0795833333333,3.64215882054307,-1.9365701964918));
#28745=CARTESIAN_POINT('Ctrl Pts',(-34.053125,4.76023814479221,0.166231178980113));
#28746=CARTESIAN_POINT('Ctrl Pts',(-34.0266666666667,3.49819839664525,2.18591696496197));
#28747=CARTESIAN_POINT('Ctrl Pts',(-34.0009587714797,2.2719539027698,4.14831836955731));
#28748=CARTESIAN_POINT('Ctrl Pts',(-33.9748916174808,-0.0419478005003553,
4.12478670745932));
#28749=CARTESIAN_POINT('Ctrl Pts',(-43.8757812504336,0.149957969249583,
-4.29423438922274));
#28750=CARTESIAN_POINT('Ctrl Pts',(-43.8493229171003,2.62923534983068,-4.20765611530936));
#28751=CARTESIAN_POINT('Ctrl Pts',(-43.8228645837669,3.79389505549643,-2.0172497837413));
#28752=CARTESIAN_POINT('Ctrl Pts',(-43.7964062504336,4.95855476116219,0.173156547826753));
#28753=CARTESIAN_POINT('Ctrl Pts',(-43.7699479171003,3.64393708624685,2.27698460548143));
#28754=CARTESIAN_POINT('Ctrl Pts',(-43.7434895837669,2.32931941133151,4.38081266313611));
#28755=CARTESIAN_POINT('Ctrl Pts',(-43.7170312504336,-0.149957969249583,
4.29423438922274));
#28756=CARTESIAN_POINT('Ctrl Pts',(-43.6905729171003,-2.62923534983068,
4.20765611530936));
#28757=CARTESIAN_POINT('Ctrl Pts',(-43.6641145837669,-3.79389505549643,
2.01724978374131));
#28758=CARTESIAN_POINT('Ctrl Pts',(-43.6376562504336,-4.95855476116219,
-0.173156547826752));
#28759=CARTESIAN_POINT('Ctrl Pts',(-43.6111979171003,-3.64393708624685,
-2.27698460548143));
#28760=CARTESIAN_POINT('Ctrl Pts',(-43.5847395837669,-2.32931941133151,
-4.38081266313611));
#28761=CARTESIAN_POINT('Ctrl Pts',(-43.5582812504336,0.149957969249583,
-4.29423438922274));
#28762=CARTESIAN_POINT('Ctrl Pts',(-43.5318229171003,2.62923534983068,-4.20765611530936));
#28763=CARTESIAN_POINT('Ctrl Pts',(-43.5053645837669,3.79389505549643,-2.0172497837413));
#28764=CARTESIAN_POINT('Ctrl Pts',(-43.4789062504336,4.95855476116219,0.173156547826753));
#28765=CARTESIAN_POINT('Ctrl Pts',(-43.4524479171003,3.64393708624685,2.27698460548143));
#28766=CARTESIAN_POINT('Ctrl Pts',(-43.4259895837669,2.32931941133151,4.38081266313611));
#28767=CARTESIAN_POINT('Ctrl Pts',(-43.3995312504336,-0.149957969249583,
4.29423438922274));
#28768=CARTESIAN_POINT('Ctrl Pts',(-43.3730729171003,-2.62923534983068,
4.20765611530936));
#28769=CARTESIAN_POINT('Ctrl Pts',(-43.3466145837669,-3.79389505549643,
2.01724978374131));
#28770=CARTESIAN_POINT('Ctrl Pts',(-43.3201562504336,-4.95855476116219,
-0.173156547826752));
#28771=CARTESIAN_POINT('Ctrl Pts',(-43.2936979171003,-3.64393708624685,
-2.27698460548143));
#28772=CARTESIAN_POINT('Ctrl Pts',(-43.2672395837669,-2.32931941133151,
-4.38081266313611));
#28773=CARTESIAN_POINT('Ctrl Pts',(-43.2407812504336,0.149957969249583,
-4.29423438922274));
#28774=CARTESIAN_POINT('Ctrl Pts',(-43.2143229171003,2.62923534983068,-4.20765611530936));
#28775=CARTESIAN_POINT('Ctrl Pts',(-43.1878645837669,3.79389505549643,-2.0172497837413));
#28776=CARTESIAN_POINT('Ctrl Pts',(-43.1614062504336,4.95855476116219,0.173156547826753));
#28777=CARTESIAN_POINT('Ctrl Pts',(-43.1349479171003,3.64393708624685,2.27698460548143));
#28778=CARTESIAN_POINT('Ctrl Pts',(-43.1084895837669,2.32931941133151,4.38081266313611));
#28779=CARTESIAN_POINT('Ctrl Pts',(-43.0820312504336,-0.149957969249583,
4.29423438922274));
#28780=CARTESIAN_POINT('Ctrl Pts',(-43.0555729171003,-2.62923534983068,
4.20765611530936));
#28781=CARTESIAN_POINT('Ctrl Pts',(-43.0291145837669,-3.79389505549643,
2.01724978374131));
#28782=CARTESIAN_POINT('Ctrl Pts',(-43.0026562504336,-4.95855476116219,
-0.173156547826752));
#28783=CARTESIAN_POINT('Ctrl Pts',(-42.9761979171003,-3.64393708624685,
-2.27698460548143));
#28784=CARTESIAN_POINT('Ctrl Pts',(-42.9497395837669,-2.32931941133151,
-4.38081266313611));
#28785=CARTESIAN_POINT('Ctrl Pts',(-42.9232812504336,0.149957969249583,
-4.29423438922274));
#28786=CARTESIAN_POINT('Ctrl Pts',(-42.8968229171003,2.62923534983068,-4.20765611530936));
#28787=CARTESIAN_POINT('Ctrl Pts',(-42.8703645837669,3.79389505549643,-2.0172497837413));
#28788=CARTESIAN_POINT('Ctrl Pts',(-42.8439062504336,4.95855476116219,0.173156547826753));
#28789=CARTESIAN_POINT('Ctrl Pts',(-42.8174479171003,3.64393708624685,2.27698460548143));
#28790=CARTESIAN_POINT('Ctrl Pts',(-42.7909895837669,2.32931941133151,4.38081266313611));
#28791=CARTESIAN_POINT('Ctrl Pts',(-42.7645312504336,-0.149957969249583,
4.29423438922274));
#28792=CARTESIAN_POINT('Ctrl Pts',(-42.7380729171003,-2.62923534983068,
4.20765611530936));
#28793=CARTESIAN_POINT('Ctrl Pts',(-42.7116145837669,-3.79389505549643,
2.01724978374131));
#28794=CARTESIAN_POINT('Ctrl Pts',(-42.6851562504336,-4.95855476116219,
-0.173156547826752));
#28795=CARTESIAN_POINT('Ctrl Pts',(-42.6586979171003,-3.64393708624685,
-2.27698460548143));
#28796=CARTESIAN_POINT('Ctrl Pts',(-42.6322395837669,-2.32931941133151,
-4.38081266313611));
#28797=CARTESIAN_POINT('Ctrl Pts',(-42.6057812504336,0.149957969249583,
-4.29423438922274));
#28798=CARTESIAN_POINT('Ctrl Pts',(-42.5793229171003,2.62923534983068,-4.20765611530936));
#28799=CARTESIAN_POINT('Ctrl Pts',(-42.5528645837669,3.79389505549643,-2.0172497837413));
#28800=CARTESIAN_POINT('Ctrl Pts',(-42.5264062504336,4.95855476116219,0.173156547826753));
#28801=CARTESIAN_POINT('Ctrl Pts',(-42.4999479171003,3.64393708624685,2.27698460548143));
#28802=CARTESIAN_POINT('Ctrl Pts',(-42.4734895837669,2.32931941133151,4.38081266313611));
#28803=CARTESIAN_POINT('Ctrl Pts',(-42.4470312504336,-0.149957969249583,
4.29423438922274));
#28804=CARTESIAN_POINT('Ctrl Pts',(-42.4205729171003,-2.62923534983068,
4.20765611530936));
#28805=CARTESIAN_POINT('Ctrl Pts',(-42.3941145837669,-3.79389505549643,
2.01724978374131));
#28806=CARTESIAN_POINT('Ctrl Pts',(-42.3676562504336,-4.95855476116219,
-0.173156547826752));
#28807=CARTESIAN_POINT('Ctrl Pts',(-42.3411979171003,-3.64393708624685,
-2.27698460548143));
#28808=CARTESIAN_POINT('Ctrl Pts',(-42.3147395837669,-2.32931941133151,
-4.38081266313611));
#28809=CARTESIAN_POINT('Ctrl Pts',(-42.2882812504336,0.149957969249583,
-4.29423438922274));
#28810=CARTESIAN_POINT('Ctrl Pts',(-42.2618229171003,2.62923534983068,-4.20765611530936));
#28811=CARTESIAN_POINT('Ctrl Pts',(-42.2353645837669,3.79389505549643,-2.0172497837413));
#28812=CARTESIAN_POINT('Ctrl Pts',(-42.2089062504336,4.95855476116219,0.173156547826753));
#28813=CARTESIAN_POINT('Ctrl Pts',(-42.1824479171003,3.64393708624685,2.27698460548143));
#28814=CARTESIAN_POINT('Ctrl Pts',(-42.1559895837669,2.32931941133151,4.38081266313611));
#28815=CARTESIAN_POINT('Ctrl Pts',(-42.1295312504336,-0.149957969249583,
4.29423438922274));
#28816=CARTESIAN_POINT('Ctrl Pts',(-42.1030729171003,-2.62923534983068,
4.20765611530936));
#28817=CARTESIAN_POINT('Ctrl Pts',(-42.0766145837669,-3.79389505549643,
2.01724978374131));
#28818=CARTESIAN_POINT('Ctrl Pts',(-42.0501562504336,-4.95855476116219,
-0.173156547826752));
#28819=CARTESIAN_POINT('Ctrl Pts',(-42.0236979171003,-3.64393708624685,
-2.27698460548143));
#28820=CARTESIAN_POINT('Ctrl Pts',(-41.9972395837669,-2.32931941133151,
-4.38081266313611));
#28821=CARTESIAN_POINT('Ctrl Pts',(-41.9707812504336,0.149957969249583,
-4.29423438922274));
#28822=CARTESIAN_POINT('Ctrl Pts',(-41.9443229171003,2.62923534983068,-4.20765611530936));
#28823=CARTESIAN_POINT('Ctrl Pts',(-41.9178645837669,3.79389505549643,-2.0172497837413));
#28824=CARTESIAN_POINT('Ctrl Pts',(-41.8914062504336,4.95855476116219,0.173156547826753));
#28825=CARTESIAN_POINT('Ctrl Pts',(-41.8649479171003,3.64393708624685,2.27698460548143));
#28826=CARTESIAN_POINT('Ctrl Pts',(-41.8384895837669,2.32931941133151,4.38081266313611));
#28827=CARTESIAN_POINT('Ctrl Pts',(-41.8120312504336,-0.149957969249583,
4.29423438922274));
#28828=CARTESIAN_POINT('Ctrl Pts',(-41.7855729171003,-2.62923534983068,
4.20765611530936));
#28829=CARTESIAN_POINT('Ctrl Pts',(-41.7591145837669,-3.79389505549643,
2.01724978374131));
#28830=CARTESIAN_POINT('Ctrl Pts',(-41.7326562504336,-4.95855476116219,
-0.173156547826752));
#28831=CARTESIAN_POINT('Ctrl Pts',(-41.7061979171003,-3.64393708624685,
-2.27698460548143));
#28832=CARTESIAN_POINT('Ctrl Pts',(-41.6797395837669,-2.32931941133151,
-4.38081266313611));
#28833=CARTESIAN_POINT('Ctrl Pts',(-41.6532812504336,0.149957969249583,
-4.29423438922274));
#28834=CARTESIAN_POINT('Ctrl Pts',(-41.6268229171003,2.62923534983068,-4.20765611530936));
#28835=CARTESIAN_POINT('Ctrl Pts',(-41.6003645837669,3.79389505549643,-2.0172497837413));
#28836=CARTESIAN_POINT('Ctrl Pts',(-41.5739062504336,4.95855476116219,0.173156547826753));
#28837=CARTESIAN_POINT('Ctrl Pts',(-41.5474479171003,3.64393708624685,2.27698460548143));
#28838=CARTESIAN_POINT('Ctrl Pts',(-41.5209895837669,2.32931941133151,4.38081266313611));
#28839=CARTESIAN_POINT('Ctrl Pts',(-41.4945312504336,-0.149957969249583,
4.29423438922274));
#28840=CARTESIAN_POINT('Ctrl Pts',(-41.4680729171003,-2.62923534983068,
4.20765611530936));
#28841=CARTESIAN_POINT('Ctrl Pts',(-41.4416145837669,-3.79389505549643,
2.01724978374131));
#28842=CARTESIAN_POINT('Ctrl Pts',(-41.4151562504336,-4.95855476116219,
-0.173156547826752));
#28843=CARTESIAN_POINT('Ctrl Pts',(-41.3886979171003,-3.64393708624685,
-2.27698460548143));
#28844=CARTESIAN_POINT('Ctrl Pts',(-41.3622395837669,-2.32931941133151,
-4.38081266313611));
#28845=CARTESIAN_POINT('Ctrl Pts',(-41.3357812504336,0.149957969249583,
-4.29423438922274));
#28846=CARTESIAN_POINT('Ctrl Pts',(-41.3093229171003,2.62923534983068,-4.20765611530936));
#28847=CARTESIAN_POINT('Ctrl Pts',(-41.2828645837669,3.79389505549643,-2.0172497837413));
#28848=CARTESIAN_POINT('Ctrl Pts',(-41.2564062504336,4.95855476116219,0.173156547826753));
#28849=CARTESIAN_POINT('Ctrl Pts',(-41.2299479171003,3.64393708624685,2.27698460548143));
#28850=CARTESIAN_POINT('Ctrl Pts',(-41.2034895837669,2.32931941133151,4.38081266313611));
#28851=CARTESIAN_POINT('Ctrl Pts',(-41.1770312504336,-0.149957969249583,
4.29423438922274));
#28852=CARTESIAN_POINT('Ctrl Pts',(-41.1505729171003,-2.62923534983068,
4.20765611530936));
#28853=CARTESIAN_POINT('Ctrl Pts',(-41.1241145837669,-3.79389505549643,
2.01724978374131));
#28854=CARTESIAN_POINT('Ctrl Pts',(-41.0976562504336,-4.95855476116219,
-0.173156547826752));
#28855=CARTESIAN_POINT('Ctrl Pts',(-41.0711979171003,-3.64393708624685,
-2.27698460548143));
#28856=CARTESIAN_POINT('Ctrl Pts',(-41.0447395837669,-2.32931941133151,
-4.38081266313611));
#28857=CARTESIAN_POINT('Ctrl Pts',(-41.0182812504336,0.149957969249583,
-4.29423438922274));
#28858=CARTESIAN_POINT('Ctrl Pts',(-40.9918229171003,2.62923534983068,-4.20765611530936));
#28859=CARTESIAN_POINT('Ctrl Pts',(-40.9653645837669,3.79389505549643,-2.0172497837413));
#28860=CARTESIAN_POINT('Ctrl Pts',(-40.9389062504336,4.95855476116219,0.173156547826753));
#28861=CARTESIAN_POINT('Ctrl Pts',(-40.9124479171003,3.64393708624685,2.27698460548143));
#28862=CARTESIAN_POINT('Ctrl Pts',(-40.8859895837669,2.32931941133151,4.38081266313611));
#28863=CARTESIAN_POINT('Ctrl Pts',(-40.8595312504336,-0.149957969249583,
4.29423438922274));
#28864=CARTESIAN_POINT('Ctrl Pts',(-40.8330729171003,-2.62923534983068,
4.20765611530936));
#28865=CARTESIAN_POINT('Ctrl Pts',(-40.8066145837669,-3.79389505549643,
2.01724978374131));
#28866=CARTESIAN_POINT('Ctrl Pts',(-40.7801562504336,-4.95855476116219,
-0.173156547826752));
#28867=CARTESIAN_POINT('Ctrl Pts',(-40.7536979171003,-3.64393708624685,
-2.27698460548143));
#28868=CARTESIAN_POINT('Ctrl Pts',(-40.7272395837669,-2.32931941133151,
-4.38081266313611));
#28869=CARTESIAN_POINT('Ctrl Pts',(-40.7007812504336,0.149957969249583,
-4.29423438922274));
#28870=CARTESIAN_POINT('Ctrl Pts',(-40.6743229171003,2.62923534983068,-4.20765611530936));
#28871=CARTESIAN_POINT('Ctrl Pts',(-40.6478645837669,3.79389505549643,-2.0172497837413));
#28872=CARTESIAN_POINT('Ctrl Pts',(-40.6214062504336,4.95855476116219,0.173156547826753));
#28873=CARTESIAN_POINT('Ctrl Pts',(-40.5949479171003,3.64393708624685,2.27698460548143));
#28874=CARTESIAN_POINT('Ctrl Pts',(-40.5684895837669,2.32931941133151,4.38081266313611));
#28875=CARTESIAN_POINT('Ctrl Pts',(-40.5420312504336,-0.149957969249583,
4.29423438922274));
#28876=CARTESIAN_POINT('Ctrl Pts',(-40.5155729171003,-2.62923534983068,
4.20765611530936));
#28877=CARTESIAN_POINT('Ctrl Pts',(-40.4891145837669,-3.79389505549643,
2.01724978374131));
#28878=CARTESIAN_POINT('Ctrl Pts',(-40.4626562504336,-4.95855476116219,
-0.173156547826752));
#28879=CARTESIAN_POINT('Ctrl Pts',(-40.4361979171003,-3.64393708624685,
-2.27698460548143));
#28880=CARTESIAN_POINT('Ctrl Pts',(-40.4097395837669,-2.32931941133151,
-4.38081266313611));
#28881=CARTESIAN_POINT('Ctrl Pts',(-40.3832812504336,0.149957969249583,
-4.29423438922274));
#28882=CARTESIAN_POINT('Ctrl Pts',(-40.3568229171003,2.62923534983068,-4.20765611530936));
#28883=CARTESIAN_POINT('Ctrl Pts',(-40.3303645837669,3.79389505549643,-2.0172497837413));
#28884=CARTESIAN_POINT('Ctrl Pts',(-40.3039062504336,4.95855476116219,0.173156547826753));
#28885=CARTESIAN_POINT('Ctrl Pts',(-40.2774479171003,3.64393708624685,2.27698460548143));
#28886=CARTESIAN_POINT('Ctrl Pts',(-40.2509895837669,2.32931941133151,4.38081266313611));
#28887=CARTESIAN_POINT('Ctrl Pts',(-40.2245312504336,-0.149957969249583,
4.29423438922274));
#28888=CARTESIAN_POINT('Ctrl Pts',(-40.1980729171003,-2.62923534983068,
4.20765611530936));
#28889=CARTESIAN_POINT('Ctrl Pts',(-40.1716145837669,-3.79389505549643,
2.01724978374131));
#28890=CARTESIAN_POINT('Ctrl Pts',(-40.1451562504336,-4.95855476116219,
-0.173156547826752));
#28891=CARTESIAN_POINT('Ctrl Pts',(-40.1186979171003,-3.64393708624685,
-2.27698460548143));
#28892=CARTESIAN_POINT('Ctrl Pts',(-40.0922395837669,-2.32931941133151,
-4.38081266313611));
#28893=CARTESIAN_POINT('Ctrl Pts',(-40.0657812504336,0.149957969249583,
-4.29423438922274));
#28894=CARTESIAN_POINT('Ctrl Pts',(-40.0393229171003,2.62923534983068,-4.20765611530936));
#28895=CARTESIAN_POINT('Ctrl Pts',(-40.0128645837669,3.79389505549643,-2.0172497837413));
#28896=CARTESIAN_POINT('Ctrl Pts',(-39.9864062504336,4.95855476116219,0.173156547826753));
#28897=CARTESIAN_POINT('Ctrl Pts',(-39.9599479171003,3.64393708624685,2.27698460548143));
#28898=CARTESIAN_POINT('Ctrl Pts',(-39.9334895837669,2.32931941133151,4.38081266313611));
#28899=CARTESIAN_POINT('Ctrl Pts',(-39.9070312504336,-0.149957969249583,
4.29423438922274));
#28900=CARTESIAN_POINT('Ctrl Pts',(-39.8805729171003,-2.62923534983068,
4.20765611530936));
#28901=CARTESIAN_POINT('Ctrl Pts',(-39.8541145837669,-3.79389505549643,
2.01724978374131));
#28902=CARTESIAN_POINT('Ctrl Pts',(-39.8276562504336,-4.95855476116219,
-0.173156547826752));
#28903=CARTESIAN_POINT('Ctrl Pts',(-39.8011979171003,-3.64393708624685,
-2.27698460548143));
#28904=CARTESIAN_POINT('Ctrl Pts',(-39.7747395837669,-2.32931941133151,
-4.38081266313611));
#28905=CARTESIAN_POINT('Ctrl Pts',(-39.7482812504336,0.149957969249583,
-4.29423438922274));
#28906=CARTESIAN_POINT('Ctrl Pts',(-39.7218229171003,2.62923534983068,-4.20765611530936));
#28907=CARTESIAN_POINT('Ctrl Pts',(-39.6953645837669,3.79389505549643,-2.0172497837413));
#28908=CARTESIAN_POINT('Ctrl Pts',(-39.6689062504336,4.95855476116219,0.173156547826753));
#28909=CARTESIAN_POINT('Ctrl Pts',(-39.6424479171003,3.64393708624685,2.27698460548143));
#28910=CARTESIAN_POINT('Ctrl Pts',(-39.6159895837669,2.32931941133151,4.38081266313611));
#28911=CARTESIAN_POINT('Ctrl Pts',(-39.5895312504336,-0.149957969249583,
4.29423438922274));
#28912=CARTESIAN_POINT('Ctrl Pts',(-39.5630729171003,-2.62923534983068,
4.20765611530936));
#28913=CARTESIAN_POINT('Ctrl Pts',(-39.5366145837669,-3.79389505549643,
2.01724978374131));
#28914=CARTESIAN_POINT('Ctrl Pts',(-39.5101562504336,-4.95855476116219,
-0.173156547826752));
#28915=CARTESIAN_POINT('Ctrl Pts',(-39.4836979171003,-3.64393708624685,
-2.27698460548143));
#28916=CARTESIAN_POINT('Ctrl Pts',(-39.4572395837669,-2.32931941133151,
-4.38081266313611));
#28917=CARTESIAN_POINT('Ctrl Pts',(-39.4307812504336,0.149957969249583,
-4.29423438922274));
#28918=CARTESIAN_POINT('Ctrl Pts',(-39.4043229171003,2.62923534983068,-4.20765611530936));
#28919=CARTESIAN_POINT('Ctrl Pts',(-39.3778645837669,3.79389505549643,-2.0172497837413));
#28920=CARTESIAN_POINT('Ctrl Pts',(-39.3514062504336,4.95855476116219,0.173156547826753));
#28921=CARTESIAN_POINT('Ctrl Pts',(-39.3249479171003,3.64393708624685,2.27698460548143));
#28922=CARTESIAN_POINT('Ctrl Pts',(-39.2984895837669,2.32931941133151,4.38081266313611));
#28923=CARTESIAN_POINT('Ctrl Pts',(-39.2720312504336,-0.149957969249583,
4.29423438922274));
#28924=CARTESIAN_POINT('Ctrl Pts',(-39.2455729171003,-2.62923534983068,
4.20765611530936));
#28925=CARTESIAN_POINT('Ctrl Pts',(-39.2191145837669,-3.79389505549643,
2.01724978374131));
#28926=CARTESIAN_POINT('Ctrl Pts',(-39.1926562504336,-4.95855476116219,
-0.173156547826752));
#28927=CARTESIAN_POINT('Ctrl Pts',(-39.1661979171003,-3.64393708624685,
-2.27698460548143));
#28928=CARTESIAN_POINT('Ctrl Pts',(-39.1397395837669,-2.32931941133151,
-4.38081266313611));
#28929=CARTESIAN_POINT('Ctrl Pts',(-39.1132812504336,0.149957969249583,
-4.29423438922274));
#28930=CARTESIAN_POINT('Ctrl Pts',(-39.0868229171003,2.62923534983068,-4.20765611530936));
#28931=CARTESIAN_POINT('Ctrl Pts',(-39.0603645837669,3.79389505549643,-2.0172497837413));
#28932=CARTESIAN_POINT('Ctrl Pts',(-39.0339062504336,4.95855476116219,0.173156547826753));
#28933=CARTESIAN_POINT('Ctrl Pts',(-39.0074479171003,3.64393708624685,2.27698460548143));
#28934=CARTESIAN_POINT('Ctrl Pts',(-38.9809895837669,2.32931941133151,4.38081266313611));
#28935=CARTESIAN_POINT('Ctrl Pts',(-38.9545312504336,-0.149957969249583,
4.29423438922274));
#28936=CARTESIAN_POINT('Ctrl Pts',(-38.9280729171003,-2.62923534983068,
4.20765611530936));
#28937=CARTESIAN_POINT('Ctrl Pts',(-38.9016145837669,-3.79389505549643,
2.01724978374131));
#28938=CARTESIAN_POINT('Ctrl Pts',(-38.8751562504336,-4.95855476116219,
-0.173156547826752));
#28939=CARTESIAN_POINT('Ctrl Pts',(-38.8486979171003,-3.64393708624685,
-2.27698460548143));
#28940=CARTESIAN_POINT('Ctrl Pts',(-38.8222395837669,-2.32931941133151,
-4.38081266313611));
#28941=CARTESIAN_POINT('Ctrl Pts',(-38.7957812504336,0.149957969249583,
-4.29423438922274));
#28942=CARTESIAN_POINT('Ctrl Pts',(-38.7693229171003,2.62923534983068,-4.20765611530936));
#28943=CARTESIAN_POINT('Ctrl Pts',(-38.7428645837669,3.79389505549643,-2.0172497837413));
#28944=CARTESIAN_POINT('Ctrl Pts',(-38.7164062504336,4.95855476116219,0.173156547826753));
#28945=CARTESIAN_POINT('Ctrl Pts',(-38.6899479171003,3.64393708624685,2.27698460548143));
#28946=CARTESIAN_POINT('Ctrl Pts',(-38.6634895837669,2.32931941133151,4.38081266313611));
#28947=CARTESIAN_POINT('Ctrl Pts',(-38.6370312504336,-0.149957969249583,
4.29423438922274));
#28948=CARTESIAN_POINT('Ctrl Pts',(-38.6105729171003,-2.62923534983068,
4.20765611530936));
#28949=CARTESIAN_POINT('Ctrl Pts',(-38.5841145837669,-3.79389505549643,
2.01724978374131));
#28950=CARTESIAN_POINT('Ctrl Pts',(-38.5576562504336,-4.95855476116219,
-0.173156547826752));
#28951=CARTESIAN_POINT('Ctrl Pts',(-38.5311979171003,-3.64393708624685,
-2.27698460548143));
#28952=CARTESIAN_POINT('Ctrl Pts',(-38.5047395837669,-2.32931941133151,
-4.38081266313611));
#28953=CARTESIAN_POINT('Ctrl Pts',(-38.4782812504336,0.149957969249583,
-4.29423438922274));
#28954=CARTESIAN_POINT('Ctrl Pts',(-38.4518229171003,2.62923534983068,-4.20765611530936));
#28955=CARTESIAN_POINT('Ctrl Pts',(-38.4253645837669,3.79389505549643,-2.0172497837413));
#28956=CARTESIAN_POINT('Ctrl Pts',(-38.3989062504336,4.95855476116219,0.173156547826753));
#28957=CARTESIAN_POINT('Ctrl Pts',(-38.3724479171003,3.64393708624685,2.27698460548143));
#28958=CARTESIAN_POINT('Ctrl Pts',(-38.3459895837669,2.32931941133151,4.38081266313611));
#28959=CARTESIAN_POINT('Ctrl Pts',(-38.3195312504336,-0.149957969249583,
4.29423438922274));
#28960=CARTESIAN_POINT('Ctrl Pts',(-38.2930729171003,-2.62923534983068,
4.20765611530936));
#28961=CARTESIAN_POINT('Ctrl Pts',(-38.2666145837669,-3.79389505549643,
2.01724978374131));
#28962=CARTESIAN_POINT('Ctrl Pts',(-38.2401562504336,-4.95855476116219,
-0.173156547826752));
#28963=CARTESIAN_POINT('Ctrl Pts',(-38.2136979171003,-3.64393708624685,
-2.27698460548143));
#28964=CARTESIAN_POINT('Ctrl Pts',(-38.1872395837669,-2.32931941133151,
-4.38081266313611));
#28965=CARTESIAN_POINT('Ctrl Pts',(-38.1607812504336,0.149957969249583,
-4.29423438922274));
#28966=CARTESIAN_POINT('Ctrl Pts',(-38.1343229171003,2.62923534983068,-4.20765611530936));
#28967=CARTESIAN_POINT('Ctrl Pts',(-38.1078645837669,3.79389505549643,-2.0172497837413));
#28968=CARTESIAN_POINT('Ctrl Pts',(-38.0814062504336,4.95855476116219,0.173156547826753));
#28969=CARTESIAN_POINT('Ctrl Pts',(-38.0549479171003,3.64393708624685,2.27698460548143));
#28970=CARTESIAN_POINT('Ctrl Pts',(-38.0284895837669,2.32931941133151,4.38081266313611));
#28971=CARTESIAN_POINT('Ctrl Pts',(-38.0020312504336,-0.149957969249583,
4.29423438922274));
#28972=CARTESIAN_POINT('Ctrl Pts',(-37.9755729171003,-2.62923534983068,
4.20765611530936));
#28973=CARTESIAN_POINT('Ctrl Pts',(-37.9491145837669,-3.79389505549643,
2.01724978374131));
#28974=CARTESIAN_POINT('Ctrl Pts',(-37.9226562504336,-4.95855476116219,
-0.173156547826752));
#28975=CARTESIAN_POINT('Ctrl Pts',(-37.8961979171003,-3.64393708624685,
-2.27698460548143));
#28976=CARTESIAN_POINT('Ctrl Pts',(-37.8697395837669,-2.32931941133151,
-4.38081266313611));
#28977=CARTESIAN_POINT('Ctrl Pts',(-37.8432812504336,0.149957969249583,
-4.29423438922274));
#28978=CARTESIAN_POINT('Ctrl Pts',(-37.8168229171003,2.62923534983068,-4.20765611530936));
#28979=CARTESIAN_POINT('Ctrl Pts',(-37.7903645837669,3.79389505549643,-2.0172497837413));
#28980=CARTESIAN_POINT('Ctrl Pts',(-37.7639062504336,4.95855476116219,0.173156547826753));
#28981=CARTESIAN_POINT('Ctrl Pts',(-37.7374479171003,3.64393708624685,2.27698460548143));
#28982=CARTESIAN_POINT('Ctrl Pts',(-37.7109895837669,2.32931941133151,4.38081266313611));
#28983=CARTESIAN_POINT('Ctrl Pts',(-37.6845312504336,-0.149957969249583,
4.29423438922274));
#28984=CARTESIAN_POINT('Ctrl Pts',(-37.6580729171003,-2.62923534983068,
4.20765611530936));
#28985=CARTESIAN_POINT('Ctrl Pts',(-37.6316145837669,-3.79389505549643,
2.01724978374131));
#28986=CARTESIAN_POINT('Ctrl Pts',(-37.6051562504336,-4.95855476116219,
-0.173156547826752));
#28987=CARTESIAN_POINT('Ctrl Pts',(-37.5786979171003,-3.64393708624685,
-2.27698460548143));
#28988=CARTESIAN_POINT('Ctrl Pts',(-37.5522395837669,-2.32931941133151,
-4.38081266313611));
#28989=CARTESIAN_POINT('Ctrl Pts',(-37.5257812504336,0.149957969249583,
-4.29423438922274));
#28990=CARTESIAN_POINT('Ctrl Pts',(-37.4993229171003,2.62923534983068,-4.20765611530936));
#28991=CARTESIAN_POINT('Ctrl Pts',(-37.4728645837669,3.79389505549643,-2.0172497837413));
#28992=CARTESIAN_POINT('Ctrl Pts',(-37.4464062504336,4.95855476116219,0.173156547826753));
#28993=CARTESIAN_POINT('Ctrl Pts',(-37.4199479171003,3.64393708624685,2.27698460548143));
#28994=CARTESIAN_POINT('Ctrl Pts',(-37.3934895837669,2.32931941133151,4.38081266313611));
#28995=CARTESIAN_POINT('Ctrl Pts',(-37.3670312504336,-0.149957969249583,
4.29423438922274));
#28996=CARTESIAN_POINT('Ctrl Pts',(-37.3405729171003,-2.62923534983068,
4.20765611530936));
#28997=CARTESIAN_POINT('Ctrl Pts',(-37.3141145837669,-3.79389505549643,
2.01724978374131));
#28998=CARTESIAN_POINT('Ctrl Pts',(-37.2876562504336,-4.95855476116219,
-0.173156547826752));
#28999=CARTESIAN_POINT('Ctrl Pts',(-37.2611979171003,-3.64393708624685,
-2.27698460548143));
#29000=CARTESIAN_POINT('Ctrl Pts',(-37.2347395837669,-2.32931941133151,
-4.38081266313611));
#29001=CARTESIAN_POINT('Ctrl Pts',(-37.2082812504336,0.149957969249583,
-4.29423438922274));
#29002=CARTESIAN_POINT('Ctrl Pts',(-37.1818229171003,2.62923534983068,-4.20765611530936));
#29003=CARTESIAN_POINT('Ctrl Pts',(-37.1553645837669,3.79389505549643,-2.0172497837413));
#29004=CARTESIAN_POINT('Ctrl Pts',(-37.1289062504336,4.95855476116219,0.173156547826753));
#29005=CARTESIAN_POINT('Ctrl Pts',(-37.1024479171003,3.64393708624685,2.27698460548143));
#29006=CARTESIAN_POINT('Ctrl Pts',(-37.0759895837669,2.32931941133151,4.38081266313611));
#29007=CARTESIAN_POINT('Ctrl Pts',(-37.0495312504336,-0.149957969249583,
4.29423438922274));
#29008=CARTESIAN_POINT('Ctrl Pts',(-37.0230729171003,-2.62923534983068,
4.20765611530936));
#29009=CARTESIAN_POINT('Ctrl Pts',(-36.9966145837669,-3.79389505549643,
2.01724978374131));
#29010=CARTESIAN_POINT('Ctrl Pts',(-36.9701562504336,-4.95855476116219,
-0.173156547826752));
#29011=CARTESIAN_POINT('Ctrl Pts',(-36.9436979171003,-3.64393708624685,
-2.27698460548143));
#29012=CARTESIAN_POINT('Ctrl Pts',(-36.9172395837669,-2.32931941133151,
-4.38081266313611));
#29013=CARTESIAN_POINT('Ctrl Pts',(-36.8907812504336,0.149957969249583,
-4.29423438922274));
#29014=CARTESIAN_POINT('Ctrl Pts',(-36.8643229171003,2.62923534983068,-4.20765611530936));
#29015=CARTESIAN_POINT('Ctrl Pts',(-36.8378645837669,3.79389505549643,-2.0172497837413));
#29016=CARTESIAN_POINT('Ctrl Pts',(-36.8114062504336,4.95855476116219,0.173156547826753));
#29017=CARTESIAN_POINT('Ctrl Pts',(-36.7849479171003,3.64393708624685,2.27698460548143));
#29018=CARTESIAN_POINT('Ctrl Pts',(-36.7584895837669,2.32931941133151,4.38081266313611));
#29019=CARTESIAN_POINT('Ctrl Pts',(-36.7320312504336,-0.149957969249583,
4.29423438922274));
#29020=CARTESIAN_POINT('Ctrl Pts',(-36.7055729171003,-2.62923534983068,
4.20765611530936));
#29021=CARTESIAN_POINT('Ctrl Pts',(-36.6791145837669,-3.79389505549643,
2.01724978374131));
#29022=CARTESIAN_POINT('Ctrl Pts',(-36.6526562504336,-4.95855476116219,
-0.173156547826752));
#29023=CARTESIAN_POINT('Ctrl Pts',(-36.6261979171003,-3.64393708624685,
-2.27698460548143));
#29024=CARTESIAN_POINT('Ctrl Pts',(-36.5997395837669,-2.32931941133151,
-4.38081266313611));
#29025=CARTESIAN_POINT('Ctrl Pts',(-36.5732812504336,0.149957969249583,
-4.29423438922274));
#29026=CARTESIAN_POINT('Ctrl Pts',(-36.5468229171003,2.62923534983068,-4.20765611530936));
#29027=CARTESIAN_POINT('Ctrl Pts',(-36.5203645837669,3.79389505549643,-2.0172497837413));
#29028=CARTESIAN_POINT('Ctrl Pts',(-36.4939062504336,4.95855476116219,0.173156547826753));
#29029=CARTESIAN_POINT('Ctrl Pts',(-36.4674479171003,3.64393708624685,2.27698460548143));
#29030=CARTESIAN_POINT('Ctrl Pts',(-36.4409895837669,2.32931941133151,4.38081266313611));
#29031=CARTESIAN_POINT('Ctrl Pts',(-36.4145312504336,-0.149957969249583,
4.29423438922274));
#29032=CARTESIAN_POINT('Ctrl Pts',(-36.3880729171003,-2.62923534983068,
4.20765611530936));
#29033=CARTESIAN_POINT('Ctrl Pts',(-36.3616145837669,-3.79389505549643,
2.01724978374131));
#29034=CARTESIAN_POINT('Ctrl Pts',(-36.3351562504336,-4.95855476116219,
-0.173156547826752));
#29035=CARTESIAN_POINT('Ctrl Pts',(-36.3086979171003,-3.64393708624685,
-2.27698460548143));
#29036=CARTESIAN_POINT('Ctrl Pts',(-36.2822395837669,-2.32931941133151,
-4.38081266313611));
#29037=CARTESIAN_POINT('Ctrl Pts',(-36.2557812504336,0.149957969249583,
-4.29423438922274));
#29038=CARTESIAN_POINT('Ctrl Pts',(-36.2293229171003,2.62923534983068,-4.20765611530936));
#29039=CARTESIAN_POINT('Ctrl Pts',(-36.2028645837669,3.79389505549643,-2.0172497837413));
#29040=CARTESIAN_POINT('Ctrl Pts',(-36.1764062504336,4.95855476116219,0.173156547826753));
#29041=CARTESIAN_POINT('Ctrl Pts',(-36.1499479171003,3.64393708624685,2.27698460548143));
#29042=CARTESIAN_POINT('Ctrl Pts',(-36.1234895837669,2.32931941133151,4.38081266313611));
#29043=CARTESIAN_POINT('Ctrl Pts',(-36.0970312504336,-0.149957969249583,
4.29423438922274));
#29044=CARTESIAN_POINT('Ctrl Pts',(-36.0705729171003,-2.62923534983068,
4.20765611530936));
#29045=CARTESIAN_POINT('Ctrl Pts',(-36.0441145837669,-3.79389505549643,
2.01724978374131));
#29046=CARTESIAN_POINT('Ctrl Pts',(-36.0176562504336,-4.95855476116219,
-0.173156547826752));
#29047=CARTESIAN_POINT('Ctrl Pts',(-35.9911979171003,-3.64393708624685,
-2.27698460548143));
#29048=CARTESIAN_POINT('Ctrl Pts',(-35.9647395837669,-2.32931941133151,
-4.38081266313611));
#29049=CARTESIAN_POINT('Ctrl Pts',(-35.9382812504336,0.149957969249583,
-4.29423438922274));
#29050=CARTESIAN_POINT('Ctrl Pts',(-35.9118229171003,2.62923534983068,-4.20765611530936));
#29051=CARTESIAN_POINT('Ctrl Pts',(-35.8853645837669,3.79389505549643,-2.0172497837413));
#29052=CARTESIAN_POINT('Ctrl Pts',(-35.8589062504336,4.95855476116219,0.173156547826753));
#29053=CARTESIAN_POINT('Ctrl Pts',(-35.8324479171003,3.64393708624685,2.27698460548143));
#29054=CARTESIAN_POINT('Ctrl Pts',(-35.8059895837669,2.32931941133151,4.38081266313611));
#29055=CARTESIAN_POINT('Ctrl Pts',(-35.7795312504336,-0.149957969249583,
4.29423438922274));
#29056=CARTESIAN_POINT('Ctrl Pts',(-35.7530729171003,-2.62923534983068,
4.20765611530936));
#29057=CARTESIAN_POINT('Ctrl Pts',(-35.7266145837669,-3.79389505549643,
2.01724978374131));
#29058=CARTESIAN_POINT('Ctrl Pts',(-35.7001562504336,-4.95855476116219,
-0.173156547826752));
#29059=CARTESIAN_POINT('Ctrl Pts',(-35.6736979171003,-3.64393708624685,
-2.27698460548143));
#29060=CARTESIAN_POINT('Ctrl Pts',(-35.6472395837669,-2.32931941133151,
-4.38081266313611));
#29061=CARTESIAN_POINT('Ctrl Pts',(-35.6207812504336,0.149957969249583,
-4.29423438922274));
#29062=CARTESIAN_POINT('Ctrl Pts',(-35.5943229171003,2.62923534983068,-4.20765611530936));
#29063=CARTESIAN_POINT('Ctrl Pts',(-35.5678645837669,3.79389505549643,-2.0172497837413));
#29064=CARTESIAN_POINT('Ctrl Pts',(-35.5414062504336,4.95855476116219,0.173156547826753));
#29065=CARTESIAN_POINT('Ctrl Pts',(-35.5149479171003,3.64393708624685,2.27698460548143));
#29066=CARTESIAN_POINT('Ctrl Pts',(-35.4884895837669,2.32931941133151,4.38081266313611));
#29067=CARTESIAN_POINT('Ctrl Pts',(-35.4620312504336,-0.149957969249583,
4.29423438922274));
#29068=CARTESIAN_POINT('Ctrl Pts',(-35.4355729171003,-2.62923534983068,
4.20765611530936));
#29069=CARTESIAN_POINT('Ctrl Pts',(-35.4091145837669,-3.79389505549643,
2.01724978374131));
#29070=CARTESIAN_POINT('Ctrl Pts',(-35.3826562504336,-4.95855476116219,
-0.173156547826752));
#29071=CARTESIAN_POINT('Ctrl Pts',(-35.3561979171003,-3.64393708624685,
-2.27698460548143));
#29072=CARTESIAN_POINT('Ctrl Pts',(-35.3297395837669,-2.32931941133151,
-4.38081266313611));
#29073=CARTESIAN_POINT('Ctrl Pts',(-35.3032812504336,0.149957969249583,
-4.29423438922274));
#29074=CARTESIAN_POINT('Ctrl Pts',(-35.2768229171003,2.62923534983068,-4.20765611530936));
#29075=CARTESIAN_POINT('Ctrl Pts',(-35.2503645837669,3.79389505549643,-2.0172497837413));
#29076=CARTESIAN_POINT('Ctrl Pts',(-35.2239062504336,4.95855476116219,0.173156547826753));
#29077=CARTESIAN_POINT('Ctrl Pts',(-35.1974479171003,3.64393708624685,2.27698460548143));
#29078=CARTESIAN_POINT('Ctrl Pts',(-35.1709895837669,2.32931941133151,4.38081266313611));
#29079=CARTESIAN_POINT('Ctrl Pts',(-35.1445312504336,-0.149957969249583,
4.29423438922274));
#29080=CARTESIAN_POINT('Ctrl Pts',(-35.1180729171003,-2.62923534983068,
4.20765611530936));
#29081=CARTESIAN_POINT('Ctrl Pts',(-35.0916145837669,-3.79389505549643,
2.01724978374131));
#29082=CARTESIAN_POINT('Ctrl Pts',(-35.0651562504336,-4.95855476116219,
-0.173156547826752));
#29083=CARTESIAN_POINT('Ctrl Pts',(-35.0386979171003,-3.64393708624685,
-2.27698460548143));
#29084=CARTESIAN_POINT('Ctrl Pts',(-35.0122395837669,-2.32931941133151,
-4.38081266313611));
#29085=CARTESIAN_POINT('Ctrl Pts',(-34.9857812504336,0.149957969249583,
-4.29423438922274));
#29086=CARTESIAN_POINT('Ctrl Pts',(-34.9593229171003,2.62923534983068,-4.20765611530936));
#29087=CARTESIAN_POINT('Ctrl Pts',(-34.9328645837669,3.79389505549643,-2.0172497837413));
#29088=CARTESIAN_POINT('Ctrl Pts',(-34.9064062504336,4.95855476116219,0.173156547826753));
#29089=CARTESIAN_POINT('Ctrl Pts',(-34.8799479171003,3.64393708624685,2.27698460548143));
#29090=CARTESIAN_POINT('Ctrl Pts',(-34.8534895837669,2.32931941133151,4.38081266313611));
#29091=CARTESIAN_POINT('Ctrl Pts',(-34.8270312504336,-0.149957969249583,
4.29423438922274));
#29092=CARTESIAN_POINT('Ctrl Pts',(-34.8005729171003,-2.62923534983068,
4.20765611530936));
#29093=CARTESIAN_POINT('Ctrl Pts',(-34.7741145837669,-3.79389505549643,
2.01724978374131));
#29094=CARTESIAN_POINT('Ctrl Pts',(-34.7476562504336,-4.95855476116219,
-0.173156547826752));
#29095=CARTESIAN_POINT('Ctrl Pts',(-34.7211979171003,-3.64393708624685,
-2.27698460548143));
#29096=CARTESIAN_POINT('Ctrl Pts',(-34.6947395837669,-2.32931941133151,
-4.38081266313611));
#29097=CARTESIAN_POINT('Ctrl Pts',(-34.6682812504336,0.149957969249583,
-4.29423438922274));
#29098=CARTESIAN_POINT('Ctrl Pts',(-34.6418229171003,2.62923534983068,-4.20765611530936));
#29099=CARTESIAN_POINT('Ctrl Pts',(-34.6153645837669,3.79389505549643,-2.0172497837413));
#29100=CARTESIAN_POINT('Ctrl Pts',(-34.5889062504336,4.95855476116219,0.173156547826753));
#29101=CARTESIAN_POINT('Ctrl Pts',(-34.5624479171003,3.64393708624685,2.27698460548143));
#29102=CARTESIAN_POINT('Ctrl Pts',(-34.5359895837669,2.32931941133151,4.38081266313611));
#29103=CARTESIAN_POINT('Ctrl Pts',(-34.5095312504336,-0.149957969249583,
4.29423438922274));
#29104=CARTESIAN_POINT('Ctrl Pts',(-34.4830729171003,-2.62923534983068,
4.20765611530936));
#29105=CARTESIAN_POINT('Ctrl Pts',(-34.4566145837669,-3.79389505549643,
2.01724978374131));
#29106=CARTESIAN_POINT('Ctrl Pts',(-34.4301562504336,-4.95855476116219,
-0.173156547826752));
#29107=CARTESIAN_POINT('Ctrl Pts',(-34.4036979171003,-3.64393708624685,
-2.27698460548143));
#29108=CARTESIAN_POINT('Ctrl Pts',(-34.3772395837669,-2.32931941133151,
-4.38081266313611));
#29109=CARTESIAN_POINT('Ctrl Pts',(-34.3507812504336,0.149957969249583,
-4.29423438922274));
#29110=CARTESIAN_POINT('Ctrl Pts',(-34.3243229171003,2.62923534983068,-4.20765611530936));
#29111=CARTESIAN_POINT('Ctrl Pts',(-34.2978645837669,3.79389505549643,-2.0172497837413));
#29112=CARTESIAN_POINT('Ctrl Pts',(-34.2714062504336,4.95855476116219,0.173156547826753));
#29113=CARTESIAN_POINT('Ctrl Pts',(-34.2449479171003,3.64393708624685,2.27698460548143));
#29114=CARTESIAN_POINT('Ctrl Pts',(-34.2184895837669,2.32931941133151,4.38081266313611));
#29115=CARTESIAN_POINT('Ctrl Pts',(-34.1920312504336,-0.149957969249583,
4.29423438922274));
#29116=CARTESIAN_POINT('Ctrl Pts',(-34.1655729171003,-2.62923534983068,
4.20765611530936));
#29117=CARTESIAN_POINT('Ctrl Pts',(-34.1391145837669,-3.79389505549643,
2.01724978374131));
#29118=CARTESIAN_POINT('Ctrl Pts',(-34.1126562504336,-4.95855476116219,
-0.173156547826752));
#29119=CARTESIAN_POINT('Ctrl Pts',(-34.0861979171003,-3.64393708624685,
-2.27698460548143));
#29120=CARTESIAN_POINT('Ctrl Pts',(-34.0597395837669,-2.32931941133151,
-4.38081266313611));
#29121=CARTESIAN_POINT('Ctrl Pts',(-34.0332812504336,0.149957969249583,
-4.29423438922274));
#29122=CARTESIAN_POINT('Ctrl Pts',(-34.0068229171003,2.62923534983068,-4.20765611530936));
#29123=CARTESIAN_POINT('Ctrl Pts',(-33.9803645837669,3.79389505549643,-2.0172497837413));
#29124=CARTESIAN_POINT('Ctrl Pts',(-33.9539062504336,4.95855476116219,0.173156547826753));
#29125=CARTESIAN_POINT('Ctrl Pts',(-33.9274479171003,3.64393708624685,2.27698460548143));
#29126=CARTESIAN_POINT('Ctrl Pts',(-33.9017400219133,2.36660593421046,4.32114175310506));
#29127=CARTESIAN_POINT('Ctrl Pts',(-33.8756728679143,-0.043695390769236,
4.29662973677627));
#29128=CARTESIAN_POINT('Ctrl Pts',(-43.8360937504336,0.149957969249583,
-4.29423438922274));
#29129=CARTESIAN_POINT('Ctrl Pts',(-43.8096354171003,2.62923534983068,-4.20765611530936));
#29130=CARTESIAN_POINT('Ctrl Pts',(-43.7831770837669,3.79389505549644,-2.0172497837413));
#29131=CARTESIAN_POINT('Ctrl Pts',(-43.7567187504336,4.95855476116219,0.173156547826753));
#29132=CARTESIAN_POINT('Ctrl Pts',(-43.7302604171003,3.64393708624685,2.27698460548143));
#29133=CARTESIAN_POINT('Ctrl Pts',(-43.7038020837669,2.32931941133151,4.38081266313611));
#29134=CARTESIAN_POINT('Ctrl Pts',(-43.6773437504336,-0.149957969249583,
4.29423438922274));
#29135=CARTESIAN_POINT('Ctrl Pts',(-43.6508854171003,-2.62923534983068,
4.20765611530936));
#29136=CARTESIAN_POINT('Ctrl Pts',(-43.6244270837669,-3.79389505549643,
2.01724978374131));
#29137=CARTESIAN_POINT('Ctrl Pts',(-43.5979687504336,-4.95855476116219,
-0.173156547826752));
#29138=CARTESIAN_POINT('Ctrl Pts',(-43.5715104171003,-3.64393708624685,
-2.27698460548143));
#29139=CARTESIAN_POINT('Ctrl Pts',(-43.5450520837669,-2.32931941133151,
-4.38081266313611));
#29140=CARTESIAN_POINT('Ctrl Pts',(-43.5185937504336,0.149957969249583,
-4.29423438922274));
#29141=CARTESIAN_POINT('Ctrl Pts',(-43.4921354171003,2.62923534983068,-4.20765611530936));
#29142=CARTESIAN_POINT('Ctrl Pts',(-43.4656770837669,3.79389505549644,-2.0172497837413));
#29143=CARTESIAN_POINT('Ctrl Pts',(-43.4392187504336,4.95855476116219,0.173156547826753));
#29144=CARTESIAN_POINT('Ctrl Pts',(-43.4127604171003,3.64393708624685,2.27698460548143));
#29145=CARTESIAN_POINT('Ctrl Pts',(-43.3863020837669,2.32931941133151,4.38081266313611));
#29146=CARTESIAN_POINT('Ctrl Pts',(-43.3598437504336,-0.149957969249583,
4.29423438922274));
#29147=CARTESIAN_POINT('Ctrl Pts',(-43.3333854171003,-2.62923534983068,
4.20765611530936));
#29148=CARTESIAN_POINT('Ctrl Pts',(-43.3069270837669,-3.79389505549643,
2.01724978374131));
#29149=CARTESIAN_POINT('Ctrl Pts',(-43.2804687504336,-4.95855476116219,
-0.173156547826752));
#29150=CARTESIAN_POINT('Ctrl Pts',(-43.2540104171003,-3.64393708624685,
-2.27698460548143));
#29151=CARTESIAN_POINT('Ctrl Pts',(-43.2275520837669,-2.32931941133151,
-4.38081266313611));
#29152=CARTESIAN_POINT('Ctrl Pts',(-43.2010937504336,0.149957969249583,
-4.29423438922274));
#29153=CARTESIAN_POINT('Ctrl Pts',(-43.1746354171003,2.62923534983068,-4.20765611530936));
#29154=CARTESIAN_POINT('Ctrl Pts',(-43.1481770837669,3.79389505549644,-2.0172497837413));
#29155=CARTESIAN_POINT('Ctrl Pts',(-43.1217187504336,4.95855476116219,0.173156547826753));
#29156=CARTESIAN_POINT('Ctrl Pts',(-43.0952604171003,3.64393708624685,2.27698460548143));
#29157=CARTESIAN_POINT('Ctrl Pts',(-43.0688020837669,2.32931941133151,4.38081266313611));
#29158=CARTESIAN_POINT('Ctrl Pts',(-43.0423437504336,-0.149957969249583,
4.29423438922274));
#29159=CARTESIAN_POINT('Ctrl Pts',(-43.0158854171003,-2.62923534983068,
4.20765611530936));
#29160=CARTESIAN_POINT('Ctrl Pts',(-42.9894270837669,-3.79389505549643,
2.01724978374131));
#29161=CARTESIAN_POINT('Ctrl Pts',(-42.9629687504336,-4.95855476116219,
-0.173156547826752));
#29162=CARTESIAN_POINT('Ctrl Pts',(-42.9365104171003,-3.64393708624685,
-2.27698460548143));
#29163=CARTESIAN_POINT('Ctrl Pts',(-42.9100520837669,-2.32931941133151,
-4.38081266313611));
#29164=CARTESIAN_POINT('Ctrl Pts',(-42.8835937504336,0.149957969249583,
-4.29423438922274));
#29165=CARTESIAN_POINT('Ctrl Pts',(-42.8571354171003,2.62923534983068,-4.20765611530936));
#29166=CARTESIAN_POINT('Ctrl Pts',(-42.8306770837669,3.79389505549644,-2.0172497837413));
#29167=CARTESIAN_POINT('Ctrl Pts',(-42.8042187504336,4.95855476116219,0.173156547826753));
#29168=CARTESIAN_POINT('Ctrl Pts',(-42.7777604171003,3.64393708624685,2.27698460548143));
#29169=CARTESIAN_POINT('Ctrl Pts',(-42.7513020837669,2.32931941133151,4.38081266313611));
#29170=CARTESIAN_POINT('Ctrl Pts',(-42.7248437504336,-0.149957969249583,
4.29423438922274));
#29171=CARTESIAN_POINT('Ctrl Pts',(-42.6983854171003,-2.62923534983068,
4.20765611530936));
#29172=CARTESIAN_POINT('Ctrl Pts',(-42.6719270837669,-3.79389505549643,
2.01724978374131));
#29173=CARTESIAN_POINT('Ctrl Pts',(-42.6454687504336,-4.95855476116219,
-0.173156547826752));
#29174=CARTESIAN_POINT('Ctrl Pts',(-42.6190104171003,-3.64393708624685,
-2.27698460548143));
#29175=CARTESIAN_POINT('Ctrl Pts',(-42.5925520837669,-2.32931941133151,
-4.38081266313611));
#29176=CARTESIAN_POINT('Ctrl Pts',(-42.5660937504336,0.149957969249583,
-4.29423438922274));
#29177=CARTESIAN_POINT('Ctrl Pts',(-42.5396354171003,2.62923534983068,-4.20765611530936));
#29178=CARTESIAN_POINT('Ctrl Pts',(-42.5131770837669,3.79389505549644,-2.0172497837413));
#29179=CARTESIAN_POINT('Ctrl Pts',(-42.4867187504336,4.95855476116219,0.173156547826753));
#29180=CARTESIAN_POINT('Ctrl Pts',(-42.4602604171003,3.64393708624685,2.27698460548143));
#29181=CARTESIAN_POINT('Ctrl Pts',(-42.4338020837669,2.32931941133151,4.38081266313611));
#29182=CARTESIAN_POINT('Ctrl Pts',(-42.4073437504336,-0.149957969249583,
4.29423438922274));
#29183=CARTESIAN_POINT('Ctrl Pts',(-42.3808854171003,-2.62923534983068,
4.20765611530936));
#29184=CARTESIAN_POINT('Ctrl Pts',(-42.3544270837669,-3.79389505549643,
2.01724978374131));
#29185=CARTESIAN_POINT('Ctrl Pts',(-42.3279687504336,-4.95855476116219,
-0.173156547826752));
#29186=CARTESIAN_POINT('Ctrl Pts',(-42.3015104171003,-3.64393708624685,
-2.27698460548143));
#29187=CARTESIAN_POINT('Ctrl Pts',(-42.2750520837669,-2.32931941133151,
-4.38081266313611));
#29188=CARTESIAN_POINT('Ctrl Pts',(-42.2485937504336,0.149957969249583,
-4.29423438922274));
#29189=CARTESIAN_POINT('Ctrl Pts',(-42.2221354171003,2.62923534983068,-4.20765611530936));
#29190=CARTESIAN_POINT('Ctrl Pts',(-42.1956770837669,3.79389505549644,-2.0172497837413));
#29191=CARTESIAN_POINT('Ctrl Pts',(-42.1692187504336,4.95855476116219,0.173156547826753));
#29192=CARTESIAN_POINT('Ctrl Pts',(-42.1427604171003,3.64393708624685,2.27698460548143));
#29193=CARTESIAN_POINT('Ctrl Pts',(-42.1163020837669,2.32931941133151,4.38081266313611));
#29194=CARTESIAN_POINT('Ctrl Pts',(-42.0898437504336,-0.149957969249583,
4.29423438922274));
#29195=CARTESIAN_POINT('Ctrl Pts',(-42.0633854171003,-2.62923534983068,
4.20765611530936));
#29196=CARTESIAN_POINT('Ctrl Pts',(-42.0369270837669,-3.79389505549643,
2.01724978374131));
#29197=CARTESIAN_POINT('Ctrl Pts',(-42.0104687504336,-4.95855476116219,
-0.173156547826752));
#29198=CARTESIAN_POINT('Ctrl Pts',(-41.9840104171003,-3.64393708624685,
-2.27698460548143));
#29199=CARTESIAN_POINT('Ctrl Pts',(-41.9575520837669,-2.32931941133151,
-4.38081266313611));
#29200=CARTESIAN_POINT('Ctrl Pts',(-41.9310937504336,0.149957969249583,
-4.29423438922274));
#29201=CARTESIAN_POINT('Ctrl Pts',(-41.9046354171003,2.62923534983068,-4.20765611530936));
#29202=CARTESIAN_POINT('Ctrl Pts',(-41.8781770837669,3.79389505549644,-2.0172497837413));
#29203=CARTESIAN_POINT('Ctrl Pts',(-41.8517187504336,4.95855476116219,0.173156547826753));
#29204=CARTESIAN_POINT('Ctrl Pts',(-41.8252604171003,3.64393708624685,2.27698460548143));
#29205=CARTESIAN_POINT('Ctrl Pts',(-41.7988020837669,2.32931941133151,4.38081266313611));
#29206=CARTESIAN_POINT('Ctrl Pts',(-41.7723437504336,-0.149957969249583,
4.29423438922274));
#29207=CARTESIAN_POINT('Ctrl Pts',(-41.7458854171003,-2.62923534983068,
4.20765611530936));
#29208=CARTESIAN_POINT('Ctrl Pts',(-41.7194270837669,-3.79389505549643,
2.01724978374131));
#29209=CARTESIAN_POINT('Ctrl Pts',(-41.6929687504336,-4.95855476116219,
-0.173156547826752));
#29210=CARTESIAN_POINT('Ctrl Pts',(-41.6665104171003,-3.64393708624685,
-2.27698460548143));
#29211=CARTESIAN_POINT('Ctrl Pts',(-41.6400520837669,-2.32931941133151,
-4.38081266313611));
#29212=CARTESIAN_POINT('Ctrl Pts',(-41.6135937504336,0.149957969249583,
-4.29423438922274));
#29213=CARTESIAN_POINT('Ctrl Pts',(-41.5871354171003,2.62923534983068,-4.20765611530936));
#29214=CARTESIAN_POINT('Ctrl Pts',(-41.5606770837669,3.79389505549644,-2.0172497837413));
#29215=CARTESIAN_POINT('Ctrl Pts',(-41.5342187504336,4.95855476116219,0.173156547826753));
#29216=CARTESIAN_POINT('Ctrl Pts',(-41.5077604171003,3.64393708624685,2.27698460548143));
#29217=CARTESIAN_POINT('Ctrl Pts',(-41.4813020837669,2.32931941133151,4.38081266313611));
#29218=CARTESIAN_POINT('Ctrl Pts',(-41.4548437504336,-0.149957969249583,
4.29423438922274));
#29219=CARTESIAN_POINT('Ctrl Pts',(-41.4283854171003,-2.62923534983068,
4.20765611530936));
#29220=CARTESIAN_POINT('Ctrl Pts',(-41.4019270837669,-3.79389505549643,
2.01724978374131));
#29221=CARTESIAN_POINT('Ctrl Pts',(-41.3754687504336,-4.95855476116219,
-0.173156547826752));
#29222=CARTESIAN_POINT('Ctrl Pts',(-41.3490104171003,-3.64393708624685,
-2.27698460548143));
#29223=CARTESIAN_POINT('Ctrl Pts',(-41.3225520837669,-2.32931941133151,
-4.38081266313611));
#29224=CARTESIAN_POINT('Ctrl Pts',(-41.2960937504336,0.149957969249583,
-4.29423438922274));
#29225=CARTESIAN_POINT('Ctrl Pts',(-41.2696354171003,2.62923534983068,-4.20765611530936));
#29226=CARTESIAN_POINT('Ctrl Pts',(-41.2431770837669,3.79389505549644,-2.0172497837413));
#29227=CARTESIAN_POINT('Ctrl Pts',(-41.2167187504336,4.95855476116219,0.173156547826753));
#29228=CARTESIAN_POINT('Ctrl Pts',(-41.1902604171003,3.64393708624685,2.27698460548143));
#29229=CARTESIAN_POINT('Ctrl Pts',(-41.1638020837669,2.32931941133151,4.38081266313611));
#29230=CARTESIAN_POINT('Ctrl Pts',(-41.1373437504336,-0.149957969249583,
4.29423438922274));
#29231=CARTESIAN_POINT('Ctrl Pts',(-41.1108854171003,-2.62923534983068,
4.20765611530936));
#29232=CARTESIAN_POINT('Ctrl Pts',(-41.0844270837669,-3.79389505549643,
2.01724978374131));
#29233=CARTESIAN_POINT('Ctrl Pts',(-41.0579687504336,-4.95855476116219,
-0.173156547826752));
#29234=CARTESIAN_POINT('Ctrl Pts',(-41.0315104171003,-3.64393708624685,
-2.27698460548143));
#29235=CARTESIAN_POINT('Ctrl Pts',(-41.0050520837669,-2.32931941133151,
-4.38081266313611));
#29236=CARTESIAN_POINT('Ctrl Pts',(-40.9785937504336,0.149957969249583,
-4.29423438922274));
#29237=CARTESIAN_POINT('Ctrl Pts',(-40.9521354171003,2.62923534983068,-4.20765611530936));
#29238=CARTESIAN_POINT('Ctrl Pts',(-40.9256770837669,3.79389505549644,-2.0172497837413));
#29239=CARTESIAN_POINT('Ctrl Pts',(-40.8992187504336,4.95855476116219,0.173156547826753));
#29240=CARTESIAN_POINT('Ctrl Pts',(-40.8727604171003,3.64393708624685,2.27698460548143));
#29241=CARTESIAN_POINT('Ctrl Pts',(-40.8463020837669,2.32931941133151,4.38081266313611));
#29242=CARTESIAN_POINT('Ctrl Pts',(-40.8198437504336,-0.149957969249583,
4.29423438922274));
#29243=CARTESIAN_POINT('Ctrl Pts',(-40.7933854171003,-2.62923534983068,
4.20765611530936));
#29244=CARTESIAN_POINT('Ctrl Pts',(-40.7669270837669,-3.79389505549643,
2.01724978374131));
#29245=CARTESIAN_POINT('Ctrl Pts',(-40.7404687504336,-4.95855476116219,
-0.173156547826752));
#29246=CARTESIAN_POINT('Ctrl Pts',(-40.7140104171003,-3.64393708624685,
-2.27698460548143));
#29247=CARTESIAN_POINT('Ctrl Pts',(-40.6875520837669,-2.32931941133151,
-4.38081266313611));
#29248=CARTESIAN_POINT('Ctrl Pts',(-40.6610937504336,0.149957969249583,
-4.29423438922274));
#29249=CARTESIAN_POINT('Ctrl Pts',(-40.6346354171003,2.62923534983068,-4.20765611530936));
#29250=CARTESIAN_POINT('Ctrl Pts',(-40.6081770837669,3.79389505549644,-2.0172497837413));
#29251=CARTESIAN_POINT('Ctrl Pts',(-40.5817187504336,4.95855476116219,0.173156547826753));
#29252=CARTESIAN_POINT('Ctrl Pts',(-40.5552604171002,3.64393708624685,2.27698460548143));
#29253=CARTESIAN_POINT('Ctrl Pts',(-40.5288020837669,2.32931941133151,4.38081266313611));
#29254=CARTESIAN_POINT('Ctrl Pts',(-40.5023437504336,-0.149957969249583,
4.29423438922274));
#29255=CARTESIAN_POINT('Ctrl Pts',(-40.4758854171003,-2.62923534983068,
4.20765611530936));
#29256=CARTESIAN_POINT('Ctrl Pts',(-40.4494270837669,-3.79389505549643,
2.01724978374131));
#29257=CARTESIAN_POINT('Ctrl Pts',(-40.4229687504336,-4.95855476116219,
-0.173156547826752));
#29258=CARTESIAN_POINT('Ctrl Pts',(-40.3965104171003,-3.64393708624685,
-2.27698460548143));
#29259=CARTESIAN_POINT('Ctrl Pts',(-40.3700520837669,-2.32931941133151,
-4.38081266313611));
#29260=CARTESIAN_POINT('Ctrl Pts',(-40.3435937504336,0.149957969249583,
-4.29423438922274));
#29261=CARTESIAN_POINT('Ctrl Pts',(-40.3171354171003,2.62923534983068,-4.20765611530936));
#29262=CARTESIAN_POINT('Ctrl Pts',(-40.2906770837669,3.79389505549644,-2.0172497837413));
#29263=CARTESIAN_POINT('Ctrl Pts',(-40.2642187504336,4.95855476116219,0.173156547826753));
#29264=CARTESIAN_POINT('Ctrl Pts',(-40.2377604171003,3.64393708624685,2.27698460548143));
#29265=CARTESIAN_POINT('Ctrl Pts',(-40.2113020837669,2.32931941133151,4.38081266313611));
#29266=CARTESIAN_POINT('Ctrl Pts',(-40.1848437504336,-0.149957969249583,
4.29423438922274));
#29267=CARTESIAN_POINT('Ctrl Pts',(-40.1583854171003,-2.62923534983068,
4.20765611530936));
#29268=CARTESIAN_POINT('Ctrl Pts',(-40.1319270837669,-3.79389505549643,
2.01724978374131));
#29269=CARTESIAN_POINT('Ctrl Pts',(-40.1054687504336,-4.95855476116219,
-0.173156547826752));
#29270=CARTESIAN_POINT('Ctrl Pts',(-40.0790104171003,-3.64393708624685,
-2.27698460548143));
#29271=CARTESIAN_POINT('Ctrl Pts',(-40.0525520837669,-2.32931941133151,
-4.38081266313611));
#29272=CARTESIAN_POINT('Ctrl Pts',(-40.0260937504336,0.149957969249583,
-4.29423438922274));
#29273=CARTESIAN_POINT('Ctrl Pts',(-39.9996354171003,2.62923534983068,-4.20765611530936));
#29274=CARTESIAN_POINT('Ctrl Pts',(-39.9731770837669,3.79389505549644,-2.0172497837413));
#29275=CARTESIAN_POINT('Ctrl Pts',(-39.9467187504336,4.95855476116219,0.173156547826753));
#29276=CARTESIAN_POINT('Ctrl Pts',(-39.9202604171003,3.64393708624685,2.27698460548143));
#29277=CARTESIAN_POINT('Ctrl Pts',(-39.8938020837669,2.32931941133151,4.38081266313611));
#29278=CARTESIAN_POINT('Ctrl Pts',(-39.8673437504336,-0.149957969249583,
4.29423438922274));
#29279=CARTESIAN_POINT('Ctrl Pts',(-39.8408854171003,-2.62923534983068,
4.20765611530936));
#29280=CARTESIAN_POINT('Ctrl Pts',(-39.8144270837669,-3.79389505549643,
2.01724978374131));
#29281=CARTESIAN_POINT('Ctrl Pts',(-39.7879687504336,-4.95855476116219,
-0.173156547826752));
#29282=CARTESIAN_POINT('Ctrl Pts',(-39.7615104171003,-3.64393708624685,
-2.27698460548143));
#29283=CARTESIAN_POINT('Ctrl Pts',(-39.7350520837669,-2.32931941133151,
-4.38081266313611));
#29284=CARTESIAN_POINT('Ctrl Pts',(-39.7085937504336,0.149957969249583,
-4.29423438922274));
#29285=CARTESIAN_POINT('Ctrl Pts',(-39.6821354171003,2.62923534983068,-4.20765611530936));
#29286=CARTESIAN_POINT('Ctrl Pts',(-39.6556770837669,3.79389505549644,-2.0172497837413));
#29287=CARTESIAN_POINT('Ctrl Pts',(-39.6292187504336,4.95855476116219,0.173156547826753));
#29288=CARTESIAN_POINT('Ctrl Pts',(-39.6027604171003,3.64393708624685,2.27698460548143));
#29289=CARTESIAN_POINT('Ctrl Pts',(-39.5763020837669,2.32931941133151,4.38081266313611));
#29290=CARTESIAN_POINT('Ctrl Pts',(-39.5498437504336,-0.149957969249583,
4.29423438922274));
#29291=CARTESIAN_POINT('Ctrl Pts',(-39.5233854171003,-2.62923534983068,
4.20765611530936));
#29292=CARTESIAN_POINT('Ctrl Pts',(-39.4969270837669,-3.79389505549643,
2.01724978374131));
#29293=CARTESIAN_POINT('Ctrl Pts',(-39.4704687504336,-4.95855476116219,
-0.173156547826752));
#29294=CARTESIAN_POINT('Ctrl Pts',(-39.4440104171003,-3.64393708624685,
-2.27698460548143));
#29295=CARTESIAN_POINT('Ctrl Pts',(-39.4175520837669,-2.32931941133151,
-4.38081266313611));
#29296=CARTESIAN_POINT('Ctrl Pts',(-39.3910937504336,0.149957969249583,
-4.29423438922274));
#29297=CARTESIAN_POINT('Ctrl Pts',(-39.3646354171003,2.62923534983068,-4.20765611530936));
#29298=CARTESIAN_POINT('Ctrl Pts',(-39.3381770837669,3.79389505549644,-2.0172497837413));
#29299=CARTESIAN_POINT('Ctrl Pts',(-39.3117187504336,4.95855476116219,0.173156547826753));
#29300=CARTESIAN_POINT('Ctrl Pts',(-39.2852604171003,3.64393708624685,2.27698460548143));
#29301=CARTESIAN_POINT('Ctrl Pts',(-39.2588020837669,2.32931941133151,4.38081266313611));
#29302=CARTESIAN_POINT('Ctrl Pts',(-39.2323437504336,-0.149957969249583,
4.29423438922274));
#29303=CARTESIAN_POINT('Ctrl Pts',(-39.2058854171003,-2.62923534983068,
4.20765611530936));
#29304=CARTESIAN_POINT('Ctrl Pts',(-39.1794270837669,-3.79389505549643,
2.01724978374131));
#29305=CARTESIAN_POINT('Ctrl Pts',(-39.1529687504336,-4.95855476116219,
-0.173156547826752));
#29306=CARTESIAN_POINT('Ctrl Pts',(-39.1265104171003,-3.64393708624685,
-2.27698460548143));
#29307=CARTESIAN_POINT('Ctrl Pts',(-39.1000520837669,-2.32931941133151,
-4.38081266313611));
#29308=CARTESIAN_POINT('Ctrl Pts',(-39.0735937504336,0.149957969249583,
-4.29423438922274));
#29309=CARTESIAN_POINT('Ctrl Pts',(-39.0471354171003,2.62923534983068,-4.20765611530936));
#29310=CARTESIAN_POINT('Ctrl Pts',(-39.0206770837669,3.79389505549644,-2.0172497837413));
#29311=CARTESIAN_POINT('Ctrl Pts',(-38.9942187504336,4.95855476116219,0.173156547826753));
#29312=CARTESIAN_POINT('Ctrl Pts',(-38.9677604171003,3.64393708624685,2.27698460548143));
#29313=CARTESIAN_POINT('Ctrl Pts',(-38.9413020837669,2.32931941133151,4.38081266313611));
#29314=CARTESIAN_POINT('Ctrl Pts',(-38.9148437504336,-0.149957969249583,
4.29423438922274));
#29315=CARTESIAN_POINT('Ctrl Pts',(-38.8883854171003,-2.62923534983068,
4.20765611530936));
#29316=CARTESIAN_POINT('Ctrl Pts',(-38.8619270837669,-3.79389505549643,
2.01724978374131));
#29317=CARTESIAN_POINT('Ctrl Pts',(-38.8354687504336,-4.95855476116219,
-0.173156547826752));
#29318=CARTESIAN_POINT('Ctrl Pts',(-38.8090104171003,-3.64393708624685,
-2.27698460548143));
#29319=CARTESIAN_POINT('Ctrl Pts',(-38.7825520837669,-2.32931941133151,
-4.38081266313611));
#29320=CARTESIAN_POINT('Ctrl Pts',(-38.7560937504336,0.149957969249583,
-4.29423438922274));
#29321=CARTESIAN_POINT('Ctrl Pts',(-38.7296354171002,2.62923534983068,-4.20765611530936));
#29322=CARTESIAN_POINT('Ctrl Pts',(-38.7031770837669,3.79389505549644,-2.0172497837413));
#29323=CARTESIAN_POINT('Ctrl Pts',(-38.6767187504336,4.95855476116219,0.173156547826753));
#29324=CARTESIAN_POINT('Ctrl Pts',(-38.6502604171003,3.64393708624685,2.27698460548143));
#29325=CARTESIAN_POINT('Ctrl Pts',(-38.6238020837669,2.32931941133151,4.38081266313611));
#29326=CARTESIAN_POINT('Ctrl Pts',(-38.5973437504336,-0.149957969249583,
4.29423438922274));
#29327=CARTESIAN_POINT('Ctrl Pts',(-38.5708854171003,-2.62923534983068,
4.20765611530936));
#29328=CARTESIAN_POINT('Ctrl Pts',(-38.5444270837669,-3.79389505549643,
2.01724978374131));
#29329=CARTESIAN_POINT('Ctrl Pts',(-38.5179687504336,-4.95855476116219,
-0.173156547826752));
#29330=CARTESIAN_POINT('Ctrl Pts',(-38.4915104171003,-3.64393708624685,
-2.27698460548143));
#29331=CARTESIAN_POINT('Ctrl Pts',(-38.4650520837669,-2.32931941133151,
-4.38081266313611));
#29332=CARTESIAN_POINT('Ctrl Pts',(-38.4385937504336,0.149957969249583,
-4.29423438922274));
#29333=CARTESIAN_POINT('Ctrl Pts',(-38.4121354171003,2.62923534983068,-4.20765611530936));
#29334=CARTESIAN_POINT('Ctrl Pts',(-38.3856770837669,3.79389505549644,-2.0172497837413));
#29335=CARTESIAN_POINT('Ctrl Pts',(-38.3592187504336,4.95855476116219,0.173156547826753));
#29336=CARTESIAN_POINT('Ctrl Pts',(-38.3327604171003,3.64393708624685,2.27698460548143));
#29337=CARTESIAN_POINT('Ctrl Pts',(-38.3063020837669,2.32931941133151,4.38081266313611));
#29338=CARTESIAN_POINT('Ctrl Pts',(-38.2798437504336,-0.149957969249583,
4.29423438922274));
#29339=CARTESIAN_POINT('Ctrl Pts',(-38.2533854171003,-2.62923534983068,
4.20765611530936));
#29340=CARTESIAN_POINT('Ctrl Pts',(-38.2269270837669,-3.79389505549643,
2.01724978374131));
#29341=CARTESIAN_POINT('Ctrl Pts',(-38.2004687504336,-4.95855476116219,
-0.173156547826752));
#29342=CARTESIAN_POINT('Ctrl Pts',(-38.1740104171002,-3.64393708624685,
-2.27698460548143));
#29343=CARTESIAN_POINT('Ctrl Pts',(-38.1475520837669,-2.32931941133151,
-4.38081266313611));
#29344=CARTESIAN_POINT('Ctrl Pts',(-38.1210937504336,0.149957969249583,
-4.29423438922274));
#29345=CARTESIAN_POINT('Ctrl Pts',(-38.0946354171003,2.62923534983068,-4.20765611530936));
#29346=CARTESIAN_POINT('Ctrl Pts',(-38.0681770837669,3.79389505549644,-2.0172497837413));
#29347=CARTESIAN_POINT('Ctrl Pts',(-38.0417187504336,4.95855476116219,0.173156547826753));
#29348=CARTESIAN_POINT('Ctrl Pts',(-38.0152604171003,3.64393708624685,2.27698460548143));
#29349=CARTESIAN_POINT('Ctrl Pts',(-37.9888020837669,2.32931941133151,4.38081266313611));
#29350=CARTESIAN_POINT('Ctrl Pts',(-37.9623437504336,-0.149957969249583,
4.29423438922274));
#29351=CARTESIAN_POINT('Ctrl Pts',(-37.9358854171003,-2.62923534983068,
4.20765611530936));
#29352=CARTESIAN_POINT('Ctrl Pts',(-37.9094270837669,-3.79389505549643,
2.01724978374131));
#29353=CARTESIAN_POINT('Ctrl Pts',(-37.8829687504336,-4.95855476116219,
-0.173156547826752));
#29354=CARTESIAN_POINT('Ctrl Pts',(-37.8565104171003,-3.64393708624685,
-2.27698460548143));
#29355=CARTESIAN_POINT('Ctrl Pts',(-37.8300520837669,-2.32931941133151,
-4.38081266313611));
#29356=CARTESIAN_POINT('Ctrl Pts',(-37.8035937504336,0.149957969249583,
-4.29423438922274));
#29357=CARTESIAN_POINT('Ctrl Pts',(-37.7771354171003,2.62923534983068,-4.20765611530936));
#29358=CARTESIAN_POINT('Ctrl Pts',(-37.7506770837669,3.79389505549644,-2.0172497837413));
#29359=CARTESIAN_POINT('Ctrl Pts',(-37.7242187504336,4.95855476116219,0.173156547826753));
#29360=CARTESIAN_POINT('Ctrl Pts',(-37.6977604171003,3.64393708624685,2.27698460548143));
#29361=CARTESIAN_POINT('Ctrl Pts',(-37.6713020837669,2.32931941133151,4.38081266313611));
#29362=CARTESIAN_POINT('Ctrl Pts',(-37.6448437504336,-0.149957969249583,
4.29423438922274));
#29363=CARTESIAN_POINT('Ctrl Pts',(-37.6183854171003,-2.62923534983068,
4.20765611530936));
#29364=CARTESIAN_POINT('Ctrl Pts',(-37.5919270837669,-3.79389505549643,
2.01724978374131));
#29365=CARTESIAN_POINT('Ctrl Pts',(-37.5654687504336,-4.95855476116219,
-0.173156547826752));
#29366=CARTESIAN_POINT('Ctrl Pts',(-37.5390104171003,-3.64393708624685,
-2.27698460548143));
#29367=CARTESIAN_POINT('Ctrl Pts',(-37.5125520837669,-2.32931941133151,
-4.38081266313611));
#29368=CARTESIAN_POINT('Ctrl Pts',(-37.4860937504336,0.149957969249583,
-4.29423438922274));
#29369=CARTESIAN_POINT('Ctrl Pts',(-37.4596354171003,2.62923534983068,-4.20765611530936));
#29370=CARTESIAN_POINT('Ctrl Pts',(-37.4331770837669,3.79389505549644,-2.0172497837413));
#29371=CARTESIAN_POINT('Ctrl Pts',(-37.4067187504336,4.95855476116219,0.173156547826753));
#29372=CARTESIAN_POINT('Ctrl Pts',(-37.3802604171003,3.64393708624685,2.27698460548143));
#29373=CARTESIAN_POINT('Ctrl Pts',(-37.3538020837669,2.32931941133151,4.38081266313611));
#29374=CARTESIAN_POINT('Ctrl Pts',(-37.3273437504336,-0.149957969249583,
4.29423438922274));
#29375=CARTESIAN_POINT('Ctrl Pts',(-37.3008854171003,-2.62923534983068,
4.20765611530936));
#29376=CARTESIAN_POINT('Ctrl Pts',(-37.2744270837669,-3.79389505549643,
2.01724978374131));
#29377=CARTESIAN_POINT('Ctrl Pts',(-37.2479687504336,-4.95855476116219,
-0.173156547826752));
#29378=CARTESIAN_POINT('Ctrl Pts',(-37.2215104171003,-3.64393708624685,
-2.27698460548143));
#29379=CARTESIAN_POINT('Ctrl Pts',(-37.1950520837669,-2.32931941133151,
-4.38081266313611));
#29380=CARTESIAN_POINT('Ctrl Pts',(-37.1685937504336,0.149957969249583,
-4.29423438922274));
#29381=CARTESIAN_POINT('Ctrl Pts',(-37.1421354171003,2.62923534983068,-4.20765611530936));
#29382=CARTESIAN_POINT('Ctrl Pts',(-37.1156770837669,3.79389505549644,-2.0172497837413));
#29383=CARTESIAN_POINT('Ctrl Pts',(-37.0892187504336,4.95855476116219,0.173156547826753));
#29384=CARTESIAN_POINT('Ctrl Pts',(-37.0627604171003,3.64393708624685,2.27698460548143));
#29385=CARTESIAN_POINT('Ctrl Pts',(-37.0363020837669,2.32931941133151,4.38081266313611));
#29386=CARTESIAN_POINT('Ctrl Pts',(-37.0098437504336,-0.149957969249583,
4.29423438922274));
#29387=CARTESIAN_POINT('Ctrl Pts',(-36.9833854171003,-2.62923534983068,
4.20765611530936));
#29388=CARTESIAN_POINT('Ctrl Pts',(-36.9569270837669,-3.79389505549643,
2.01724978374131));
#29389=CARTESIAN_POINT('Ctrl Pts',(-36.9304687504336,-4.95855476116219,
-0.173156547826752));
#29390=CARTESIAN_POINT('Ctrl Pts',(-36.9040104171003,-3.64393708624685,
-2.27698460548143));
#29391=CARTESIAN_POINT('Ctrl Pts',(-36.8775520837669,-2.32931941133151,
-4.38081266313611));
#29392=CARTESIAN_POINT('Ctrl Pts',(-36.8510937504336,0.149957969249583,
-4.29423438922274));
#29393=CARTESIAN_POINT('Ctrl Pts',(-36.8246354171003,2.62923534983068,-4.20765611530936));
#29394=CARTESIAN_POINT('Ctrl Pts',(-36.7981770837669,3.79389505549644,-2.0172497837413));
#29395=CARTESIAN_POINT('Ctrl Pts',(-36.7717187504336,4.95855476116219,0.173156547826753));
#29396=CARTESIAN_POINT('Ctrl Pts',(-36.7452604171003,3.64393708624685,2.27698460548143));
#29397=CARTESIAN_POINT('Ctrl Pts',(-36.7188020837669,2.32931941133151,4.38081266313611));
#29398=CARTESIAN_POINT('Ctrl Pts',(-36.6923437504336,-0.149957969249583,
4.29423438922274));
#29399=CARTESIAN_POINT('Ctrl Pts',(-36.6658854171003,-2.62923534983068,
4.20765611530936));
#29400=CARTESIAN_POINT('Ctrl Pts',(-36.6394270837669,-3.79389505549643,
2.01724978374131));
#29401=CARTESIAN_POINT('Ctrl Pts',(-36.6129687504336,-4.95855476116219,
-0.173156547826752));
#29402=CARTESIAN_POINT('Ctrl Pts',(-36.5865104171002,-3.64393708624685,
-2.27698460548143));
#29403=CARTESIAN_POINT('Ctrl Pts',(-36.5600520837669,-2.32931941133151,
-4.38081266313611));
#29404=CARTESIAN_POINT('Ctrl Pts',(-36.5335937504336,0.149957969249583,
-4.29423438922274));
#29405=CARTESIAN_POINT('Ctrl Pts',(-36.5071354171003,2.62923534983068,-4.20765611530936));
#29406=CARTESIAN_POINT('Ctrl Pts',(-36.4806770837669,3.79389505549644,-2.0172497837413));
#29407=CARTESIAN_POINT('Ctrl Pts',(-36.4542187504336,4.95855476116219,0.173156547826753));
#29408=CARTESIAN_POINT('Ctrl Pts',(-36.4277604171003,3.64393708624685,2.27698460548143));
#29409=CARTESIAN_POINT('Ctrl Pts',(-36.4013020837669,2.32931941133151,4.38081266313611));
#29410=CARTESIAN_POINT('Ctrl Pts',(-36.3748437504336,-0.149957969249583,
4.29423438922274));
#29411=CARTESIAN_POINT('Ctrl Pts',(-36.3483854171003,-2.62923534983068,
4.20765611530936));
#29412=CARTESIAN_POINT('Ctrl Pts',(-36.3219270837669,-3.79389505549643,
2.01724978374131));
#29413=CARTESIAN_POINT('Ctrl Pts',(-36.2954687504336,-4.95855476116219,
-0.173156547826752));
#29414=CARTESIAN_POINT('Ctrl Pts',(-36.2690104171003,-3.64393708624685,
-2.27698460548143));
#29415=CARTESIAN_POINT('Ctrl Pts',(-36.2425520837669,-2.32931941133151,
-4.38081266313611));
#29416=CARTESIAN_POINT('Ctrl Pts',(-36.2160937504336,0.149957969249583,
-4.29423438922274));
#29417=CARTESIAN_POINT('Ctrl Pts',(-36.1896354171003,2.62923534983068,-4.20765611530936));
#29418=CARTESIAN_POINT('Ctrl Pts',(-36.1631770837669,3.79389505549644,-2.0172497837413));
#29419=CARTESIAN_POINT('Ctrl Pts',(-36.1367187504336,4.95855476116219,0.173156547826753));
#29420=CARTESIAN_POINT('Ctrl Pts',(-36.1102604171003,3.64393708624685,2.27698460548143));
#29421=CARTESIAN_POINT('Ctrl Pts',(-36.0838020837669,2.32931941133151,4.38081266313611));
#29422=CARTESIAN_POINT('Ctrl Pts',(-36.0573437504336,-0.149957969249583,
4.29423438922274));
#29423=CARTESIAN_POINT('Ctrl Pts',(-36.0308854171003,-2.62923534983068,
4.20765611530936));
#29424=CARTESIAN_POINT('Ctrl Pts',(-36.0044270837669,-3.79389505549643,
2.01724978374131));
#29425=CARTESIAN_POINT('Ctrl Pts',(-35.9779687504336,-4.95855476116219,
-0.173156547826752));
#29426=CARTESIAN_POINT('Ctrl Pts',(-35.9515104171003,-3.64393708624685,
-2.27698460548143));
#29427=CARTESIAN_POINT('Ctrl Pts',(-35.9250520837669,-2.32931941133151,
-4.38081266313611));
#29428=CARTESIAN_POINT('Ctrl Pts',(-35.8985937504336,0.149957969249583,
-4.29423438922274));
#29429=CARTESIAN_POINT('Ctrl Pts',(-35.8721354171003,2.62923534983068,-4.20765611530936));
#29430=CARTESIAN_POINT('Ctrl Pts',(-35.8456770837669,3.79389505549644,-2.0172497837413));
#29431=CARTESIAN_POINT('Ctrl Pts',(-35.8192187504336,4.95855476116219,0.173156547826753));
#29432=CARTESIAN_POINT('Ctrl Pts',(-35.7927604171002,3.64393708624685,2.27698460548143));
#29433=CARTESIAN_POINT('Ctrl Pts',(-35.7663020837669,2.32931941133151,4.38081266313611));
#29434=CARTESIAN_POINT('Ctrl Pts',(-35.7398437504336,-0.149957969249583,
4.29423438922274));
#29435=CARTESIAN_POINT('Ctrl Pts',(-35.7133854171003,-2.62923534983068,
4.20765611530936));
#29436=CARTESIAN_POINT('Ctrl Pts',(-35.6869270837669,-3.79389505549643,
2.01724978374131));
#29437=CARTESIAN_POINT('Ctrl Pts',(-35.6604687504336,-4.95855476116219,
-0.173156547826752));
#29438=CARTESIAN_POINT('Ctrl Pts',(-35.6340104171002,-3.64393708624685,
-2.27698460548143));
#29439=CARTESIAN_POINT('Ctrl Pts',(-35.6075520837669,-2.32931941133151,
-4.38081266313611));
#29440=CARTESIAN_POINT('Ctrl Pts',(-35.5810937504336,0.149957969249583,
-4.29423438922274));
#29441=CARTESIAN_POINT('Ctrl Pts',(-35.5546354171003,2.62923534983068,-4.20765611530936));
#29442=CARTESIAN_POINT('Ctrl Pts',(-35.5281770837669,3.79389505549644,-2.0172497837413));
#29443=CARTESIAN_POINT('Ctrl Pts',(-35.5017187504336,4.95855476116219,0.173156547826753));
#29444=CARTESIAN_POINT('Ctrl Pts',(-35.4752604171003,3.64393708624685,2.27698460548143));
#29445=CARTESIAN_POINT('Ctrl Pts',(-35.4488020837669,2.32931941133151,4.38081266313611));
#29446=CARTESIAN_POINT('Ctrl Pts',(-35.4223437504336,-0.149957969249583,
4.29423438922274));
#29447=CARTESIAN_POINT('Ctrl Pts',(-35.3958854171003,-2.62923534983068,
4.20765611530936));
#29448=CARTESIAN_POINT('Ctrl Pts',(-35.3694270837669,-3.79389505549643,
2.01724978374131));
#29449=CARTESIAN_POINT('Ctrl Pts',(-35.3429687504336,-4.95855476116219,
-0.173156547826752));
#29450=CARTESIAN_POINT('Ctrl Pts',(-35.3165104171003,-3.64393708624685,
-2.27698460548143));
#29451=CARTESIAN_POINT('Ctrl Pts',(-35.2900520837669,-2.32931941133151,
-4.38081266313611));
#29452=CARTESIAN_POINT('Ctrl Pts',(-35.2635937504336,0.149957969249583,
-4.29423438922274));
#29453=CARTESIAN_POINT('Ctrl Pts',(-35.2371354171003,2.62923534983068,-4.20765611530936));
#29454=CARTESIAN_POINT('Ctrl Pts',(-35.2106770837669,3.79389505549644,-2.0172497837413));
#29455=CARTESIAN_POINT('Ctrl Pts',(-35.1842187504336,4.95855476116219,0.173156547826753));
#29456=CARTESIAN_POINT('Ctrl Pts',(-35.1577604171003,3.64393708624685,2.27698460548143));
#29457=CARTESIAN_POINT('Ctrl Pts',(-35.1313020837669,2.32931941133151,4.38081266313611));
#29458=CARTESIAN_POINT('Ctrl Pts',(-35.1048437504336,-0.149957969249583,
4.29423438922274));
#29459=CARTESIAN_POINT('Ctrl Pts',(-35.0783854171003,-2.62923534983068,
4.20765611530936));
#29460=CARTESIAN_POINT('Ctrl Pts',(-35.0519270837669,-3.79389505549643,
2.01724978374131));
#29461=CARTESIAN_POINT('Ctrl Pts',(-35.0254687504336,-4.95855476116219,
-0.173156547826752));
#29462=CARTESIAN_POINT('Ctrl Pts',(-34.9990104171003,-3.64393708624685,
-2.27698460548143));
#29463=CARTESIAN_POINT('Ctrl Pts',(-34.9725520837669,-2.32931941133151,
-4.38081266313611));
#29464=CARTESIAN_POINT('Ctrl Pts',(-34.9460937504336,0.149957969249583,
-4.29423438922274));
#29465=CARTESIAN_POINT('Ctrl Pts',(-34.9196354171003,2.62923534983068,-4.20765611530936));
#29466=CARTESIAN_POINT('Ctrl Pts',(-34.8931770837669,3.79389505549644,-2.0172497837413));
#29467=CARTESIAN_POINT('Ctrl Pts',(-34.8667187504336,4.95855476116219,0.173156547826753));
#29468=CARTESIAN_POINT('Ctrl Pts',(-34.8402604171003,3.64393708624685,2.27698460548143));
#29469=CARTESIAN_POINT('Ctrl Pts',(-34.8138020837669,2.32931941133151,4.38081266313611));
#29470=CARTESIAN_POINT('Ctrl Pts',(-34.7873437504336,-0.149957969249583,
4.29423438922274));
#29471=CARTESIAN_POINT('Ctrl Pts',(-34.7608854171003,-2.62923534983068,
4.20765611530936));
#29472=CARTESIAN_POINT('Ctrl Pts',(-34.7344270837669,-3.79389505549643,
2.01724978374131));
#29473=CARTESIAN_POINT('Ctrl Pts',(-34.7079687504336,-4.95855476116219,
-0.173156547826752));
#29474=CARTESIAN_POINT('Ctrl Pts',(-34.6815104171003,-3.64393708624685,
-2.27698460548143));
#29475=CARTESIAN_POINT('Ctrl Pts',(-34.6550520837669,-2.32931941133151,
-4.38081266313611));
#29476=CARTESIAN_POINT('Ctrl Pts',(-34.6285937504336,0.149957969249583,
-4.29423438922274));
#29477=CARTESIAN_POINT('Ctrl Pts',(-34.6021354171003,2.62923534983068,-4.20765611530936));
#29478=CARTESIAN_POINT('Ctrl Pts',(-34.5756770837669,3.79389505549644,-2.0172497837413));
#29479=CARTESIAN_POINT('Ctrl Pts',(-34.5492187504336,4.95855476116219,0.173156547826753));
#29480=CARTESIAN_POINT('Ctrl Pts',(-34.5227604171003,3.64393708624685,2.27698460548143));
#29481=CARTESIAN_POINT('Ctrl Pts',(-34.4963020837669,2.32931941133151,4.38081266313611));
#29482=CARTESIAN_POINT('Ctrl Pts',(-34.4698437504336,-0.149957969249583,
4.29423438922274));
#29483=CARTESIAN_POINT('Ctrl Pts',(-34.4433854171002,-2.62923534983068,
4.20765611530936));
#29484=CARTESIAN_POINT('Ctrl Pts',(-34.4169270837669,-3.79389505549643,
2.01724978374131));
#29485=CARTESIAN_POINT('Ctrl Pts',(-34.3904687504336,-4.95855476116219,
-0.173156547826752));
#29486=CARTESIAN_POINT('Ctrl Pts',(-34.3640104171003,-3.64393708624685,
-2.27698460548143));
#29487=CARTESIAN_POINT('Ctrl Pts',(-34.3375520837669,-2.32931941133151,
-4.38081266313611));
#29488=CARTESIAN_POINT('Ctrl Pts',(-34.3110937504336,0.149957969249583,
-4.29423438922274));
#29489=CARTESIAN_POINT('Ctrl Pts',(-34.2846354171002,2.62923534983068,-4.20765611530936));
#29490=CARTESIAN_POINT('Ctrl Pts',(-34.2581770837669,3.79389505549644,-2.0172497837413));
#29491=CARTESIAN_POINT('Ctrl Pts',(-34.2317187504336,4.95855476116219,0.173156547826753));
#29492=CARTESIAN_POINT('Ctrl Pts',(-34.2052604171002,3.64393708624685,2.27698460548143));
#29493=CARTESIAN_POINT('Ctrl Pts',(-34.1788020837669,2.32931941133151,4.38081266313611));
#29494=CARTESIAN_POINT('Ctrl Pts',(-34.1523437504336,-0.149957969249583,
4.29423438922274));
#29495=CARTESIAN_POINT('Ctrl Pts',(-34.1258854171002,-2.62923534983068,
4.20765611530936));
#29496=CARTESIAN_POINT('Ctrl Pts',(-34.0994270837669,-3.79389505549643,
2.01724978374131));
#29497=CARTESIAN_POINT('Ctrl Pts',(-34.0729687504336,-4.95855476116219,
-0.173156547826752));
#29498=CARTESIAN_POINT('Ctrl Pts',(-34.0465104171003,-3.64393708624685,
-2.27698460548143));
#29499=CARTESIAN_POINT('Ctrl Pts',(-34.0200520837669,-2.32931941133151,
-4.38081266313611));
#29500=CARTESIAN_POINT('Ctrl Pts',(-33.9935937504336,0.149957969249583,
-4.29423438922274));
#29501=CARTESIAN_POINT('Ctrl Pts',(-33.9671354171003,2.62923534983068,-4.20765611530936));
#29502=CARTESIAN_POINT('Ctrl Pts',(-33.9406770837669,3.79389505549644,-2.0172497837413));
#29503=CARTESIAN_POINT('Ctrl Pts',(-33.9142187504336,4.95855476116219,0.173156547826753));
#29504=CARTESIAN_POINT('Ctrl Pts',(-33.8877604171003,3.64393708624685,2.27698460548143));
#29505=CARTESIAN_POINT('Ctrl Pts',(-33.8620525212145,2.36660589948903,4.32114180867095));
#29506=CARTESIAN_POINT('Ctrl Pts',(-33.8359853668364,-0.0436954904407579,
4.29662973576265));
#29507=CARTESIAN_POINT('Ctrl Pts',(-43.7368750008672,0.143960423897816,
-4.12248716145376));
#29508=CARTESIAN_POINT('Ctrl Pts',(-43.7104166675338,2.52407949629392,-4.03937157196371));
#29509=CARTESIAN_POINT('Ctrl Pts',(-43.6839583342005,3.64215882054307,-1.9365701964918));
#29510=CARTESIAN_POINT('Ctrl Pts',(-43.6575000008672,4.76023814479221,0.166231178980113));
#29511=CARTESIAN_POINT('Ctrl Pts',(-43.6310416675338,3.49819839664525,2.18591696496197));
#29512=CARTESIAN_POINT('Ctrl Pts',(-43.6045833342005,2.23615864849829,4.20560275094382));
#29513=CARTESIAN_POINT('Ctrl Pts',(-43.5781250008672,-0.143960423897816,
4.12248716145376));
#29514=CARTESIAN_POINT('Ctrl Pts',(-43.5516666675338,-2.52407949629392,
4.03937157196371));
#29515=CARTESIAN_POINT('Ctrl Pts',(-43.5252083342005,-3.64215882054307,
1.9365701964918));
#29516=CARTESIAN_POINT('Ctrl Pts',(-43.4987500008672,-4.76023814479221,
-0.166231178980113));
#29517=CARTESIAN_POINT('Ctrl Pts',(-43.4722916675338,-3.49819839664525,
-2.18591696496196));
#29518=CARTESIAN_POINT('Ctrl Pts',(-43.4458333342005,-2.23615864849829,
-4.20560275094382));
#29519=CARTESIAN_POINT('Ctrl Pts',(-43.4193750008672,0.143960423897816,
-4.12248716145376));
#29520=CARTESIAN_POINT('Ctrl Pts',(-43.3929166675338,2.52407949629392,-4.03937157196371));
#29521=CARTESIAN_POINT('Ctrl Pts',(-43.3664583342005,3.64215882054307,-1.9365701964918));
#29522=CARTESIAN_POINT('Ctrl Pts',(-43.3400000008672,4.76023814479221,0.166231178980113));
#29523=CARTESIAN_POINT('Ctrl Pts',(-43.3135416675338,3.49819839664525,2.18591696496197));
#29524=CARTESIAN_POINT('Ctrl Pts',(-43.2870833342005,2.23615864849829,4.20560275094382));
#29525=CARTESIAN_POINT('Ctrl Pts',(-43.2606250008672,-0.143960423897816,
4.12248716145376));
#29526=CARTESIAN_POINT('Ctrl Pts',(-43.2341666675338,-2.52407949629392,
4.03937157196371));
#29527=CARTESIAN_POINT('Ctrl Pts',(-43.2077083342005,-3.64215882054307,
1.9365701964918));
#29528=CARTESIAN_POINT('Ctrl Pts',(-43.1812500008672,-4.76023814479221,
-0.166231178980113));
#29529=CARTESIAN_POINT('Ctrl Pts',(-43.1547916675338,-3.49819839664525,
-2.18591696496196));
#29530=CARTESIAN_POINT('Ctrl Pts',(-43.1283333342005,-2.23615864849829,
-4.20560275094382));
#29531=CARTESIAN_POINT('Ctrl Pts',(-43.1018750008672,0.143960423897816,
-4.12248716145376));
#29532=CARTESIAN_POINT('Ctrl Pts',(-43.0754166675338,2.52407949629392,-4.03937157196371));
#29533=CARTESIAN_POINT('Ctrl Pts',(-43.0489583342005,3.64215882054307,-1.9365701964918));
#29534=CARTESIAN_POINT('Ctrl Pts',(-43.0225000008672,4.76023814479221,0.166231178980113));
#29535=CARTESIAN_POINT('Ctrl Pts',(-42.9960416675338,3.49819839664525,2.18591696496197));
#29536=CARTESIAN_POINT('Ctrl Pts',(-42.9695833342005,2.23615864849829,4.20560275094382));
#29537=CARTESIAN_POINT('Ctrl Pts',(-42.9431250008672,-0.143960423897816,
4.12248716145376));
#29538=CARTESIAN_POINT('Ctrl Pts',(-42.9166666675338,-2.52407949629392,
4.03937157196371));
#29539=CARTESIAN_POINT('Ctrl Pts',(-42.8902083342005,-3.64215882054307,
1.9365701964918));
#29540=CARTESIAN_POINT('Ctrl Pts',(-42.8637500008672,-4.76023814479221,
-0.166231178980113));
#29541=CARTESIAN_POINT('Ctrl Pts',(-42.8372916675338,-3.49819839664525,
-2.18591696496196));
#29542=CARTESIAN_POINT('Ctrl Pts',(-42.8108333342005,-2.23615864849829,
-4.20560275094382));
#29543=CARTESIAN_POINT('Ctrl Pts',(-42.7843750008672,0.143960423897816,
-4.12248716145376));
#29544=CARTESIAN_POINT('Ctrl Pts',(-42.7579166675338,2.52407949629392,-4.03937157196371));
#29545=CARTESIAN_POINT('Ctrl Pts',(-42.7314583342005,3.64215882054307,-1.9365701964918));
#29546=CARTESIAN_POINT('Ctrl Pts',(-42.7050000008672,4.76023814479221,0.166231178980113));
#29547=CARTESIAN_POINT('Ctrl Pts',(-42.6785416675338,3.49819839664525,2.18591696496197));
#29548=CARTESIAN_POINT('Ctrl Pts',(-42.6520833342005,2.23615864849829,4.20560275094382));
#29549=CARTESIAN_POINT('Ctrl Pts',(-42.6256250008672,-0.143960423897816,
4.12248716145376));
#29550=CARTESIAN_POINT('Ctrl Pts',(-42.5991666675338,-2.52407949629392,
4.03937157196371));
#29551=CARTESIAN_POINT('Ctrl Pts',(-42.5727083342005,-3.64215882054307,
1.9365701964918));
#29552=CARTESIAN_POINT('Ctrl Pts',(-42.5462500008672,-4.76023814479221,
-0.166231178980113));
#29553=CARTESIAN_POINT('Ctrl Pts',(-42.5197916675338,-3.49819839664525,
-2.18591696496196));
#29554=CARTESIAN_POINT('Ctrl Pts',(-42.4933333342005,-2.23615864849829,
-4.20560275094382));
#29555=CARTESIAN_POINT('Ctrl Pts',(-42.4668750008672,0.143960423897816,
-4.12248716145376));
#29556=CARTESIAN_POINT('Ctrl Pts',(-42.4404166675338,2.52407949629392,-4.03937157196371));
#29557=CARTESIAN_POINT('Ctrl Pts',(-42.4139583342005,3.64215882054307,-1.9365701964918));
#29558=CARTESIAN_POINT('Ctrl Pts',(-42.3875000008672,4.76023814479221,0.166231178980113));
#29559=CARTESIAN_POINT('Ctrl Pts',(-42.3610416675338,3.49819839664525,2.18591696496197));
#29560=CARTESIAN_POINT('Ctrl Pts',(-42.3345833342005,2.23615864849829,4.20560275094382));
#29561=CARTESIAN_POINT('Ctrl Pts',(-42.3081250008672,-0.143960423897816,
4.12248716145376));
#29562=CARTESIAN_POINT('Ctrl Pts',(-42.2816666675338,-2.52407949629392,
4.03937157196371));
#29563=CARTESIAN_POINT('Ctrl Pts',(-42.2552083342005,-3.64215882054307,
1.9365701964918));
#29564=CARTESIAN_POINT('Ctrl Pts',(-42.2287500008672,-4.76023814479221,
-0.166231178980113));
#29565=CARTESIAN_POINT('Ctrl Pts',(-42.2022916675338,-3.49819839664525,
-2.18591696496196));
#29566=CARTESIAN_POINT('Ctrl Pts',(-42.1758333342005,-2.23615864849829,
-4.20560275094382));
#29567=CARTESIAN_POINT('Ctrl Pts',(-42.1493750008672,0.143960423897816,
-4.12248716145376));
#29568=CARTESIAN_POINT('Ctrl Pts',(-42.1229166675338,2.52407949629392,-4.03937157196371));
#29569=CARTESIAN_POINT('Ctrl Pts',(-42.0964583342005,3.64215882054307,-1.9365701964918));
#29570=CARTESIAN_POINT('Ctrl Pts',(-42.0700000008672,4.76023814479221,0.166231178980113));
#29571=CARTESIAN_POINT('Ctrl Pts',(-42.0435416675338,3.49819839664525,2.18591696496197));
#29572=CARTESIAN_POINT('Ctrl Pts',(-42.0170833342005,2.23615864849829,4.20560275094382));
#29573=CARTESIAN_POINT('Ctrl Pts',(-41.9906250008672,-0.143960423897816,
4.12248716145376));
#29574=CARTESIAN_POINT('Ctrl Pts',(-41.9641666675338,-2.52407949629392,
4.03937157196371));
#29575=CARTESIAN_POINT('Ctrl Pts',(-41.9377083342005,-3.64215882054307,
1.9365701964918));
#29576=CARTESIAN_POINT('Ctrl Pts',(-41.9112500008672,-4.76023814479221,
-0.166231178980113));
#29577=CARTESIAN_POINT('Ctrl Pts',(-41.8847916675338,-3.49819839664525,
-2.18591696496196));
#29578=CARTESIAN_POINT('Ctrl Pts',(-41.8583333342005,-2.23615864849829,
-4.20560275094382));
#29579=CARTESIAN_POINT('Ctrl Pts',(-41.8318750008672,0.143960423897816,
-4.12248716145376));
#29580=CARTESIAN_POINT('Ctrl Pts',(-41.8054166675338,2.52407949629392,-4.03937157196371));
#29581=CARTESIAN_POINT('Ctrl Pts',(-41.7789583342005,3.64215882054307,-1.9365701964918));
#29582=CARTESIAN_POINT('Ctrl Pts',(-41.7525000008672,4.76023814479221,0.166231178980113));
#29583=CARTESIAN_POINT('Ctrl Pts',(-41.7260416675338,3.49819839664525,2.18591696496197));
#29584=CARTESIAN_POINT('Ctrl Pts',(-41.6995833342005,2.23615864849829,4.20560275094382));
#29585=CARTESIAN_POINT('Ctrl Pts',(-41.6731250008672,-0.143960423897816,
4.12248716145376));
#29586=CARTESIAN_POINT('Ctrl Pts',(-41.6466666675338,-2.52407949629392,
4.03937157196371));
#29587=CARTESIAN_POINT('Ctrl Pts',(-41.6202083342005,-3.64215882054307,
1.9365701964918));
#29588=CARTESIAN_POINT('Ctrl Pts',(-41.5937500008672,-4.76023814479221,
-0.166231178980113));
#29589=CARTESIAN_POINT('Ctrl Pts',(-41.5672916675338,-3.49819839664525,
-2.18591696496196));
#29590=CARTESIAN_POINT('Ctrl Pts',(-41.5408333342005,-2.23615864849829,
-4.20560275094382));
#29591=CARTESIAN_POINT('Ctrl Pts',(-41.5143750008672,0.143960423897816,
-4.12248716145376));
#29592=CARTESIAN_POINT('Ctrl Pts',(-41.4879166675338,2.52407949629392,-4.03937157196371));
#29593=CARTESIAN_POINT('Ctrl Pts',(-41.4614583342005,3.64215882054307,-1.9365701964918));
#29594=CARTESIAN_POINT('Ctrl Pts',(-41.4350000008672,4.76023814479221,0.166231178980113));
#29595=CARTESIAN_POINT('Ctrl Pts',(-41.4085416675338,3.49819839664525,2.18591696496197));
#29596=CARTESIAN_POINT('Ctrl Pts',(-41.3820833342005,2.23615864849829,4.20560275094382));
#29597=CARTESIAN_POINT('Ctrl Pts',(-41.3556250008672,-0.143960423897816,
4.12248716145376));
#29598=CARTESIAN_POINT('Ctrl Pts',(-41.3291666675338,-2.52407949629392,
4.03937157196371));
#29599=CARTESIAN_POINT('Ctrl Pts',(-41.3027083342005,-3.64215882054307,
1.9365701964918));
#29600=CARTESIAN_POINT('Ctrl Pts',(-41.2762500008672,-4.76023814479221,
-0.166231178980113));
#29601=CARTESIAN_POINT('Ctrl Pts',(-41.2497916675338,-3.49819839664525,
-2.18591696496196));
#29602=CARTESIAN_POINT('Ctrl Pts',(-41.2233333342005,-2.23615864849829,
-4.20560275094382));
#29603=CARTESIAN_POINT('Ctrl Pts',(-41.1968750008672,0.143960423897816,
-4.12248716145376));
#29604=CARTESIAN_POINT('Ctrl Pts',(-41.1704166675338,2.52407949629392,-4.03937157196371));
#29605=CARTESIAN_POINT('Ctrl Pts',(-41.1439583342005,3.64215882054307,-1.9365701964918));
#29606=CARTESIAN_POINT('Ctrl Pts',(-41.1175000008672,4.76023814479221,0.166231178980113));
#29607=CARTESIAN_POINT('Ctrl Pts',(-41.0910416675338,3.49819839664525,2.18591696496197));
#29608=CARTESIAN_POINT('Ctrl Pts',(-41.0645833342005,2.23615864849829,4.20560275094382));
#29609=CARTESIAN_POINT('Ctrl Pts',(-41.0381250008672,-0.143960423897816,
4.12248716145376));
#29610=CARTESIAN_POINT('Ctrl Pts',(-41.0116666675338,-2.52407949629392,
4.03937157196371));
#29611=CARTESIAN_POINT('Ctrl Pts',(-40.9852083342005,-3.64215882054307,
1.9365701964918));
#29612=CARTESIAN_POINT('Ctrl Pts',(-40.9587500008672,-4.76023814479221,
-0.166231178980113));
#29613=CARTESIAN_POINT('Ctrl Pts',(-40.9322916675338,-3.49819839664525,
-2.18591696496196));
#29614=CARTESIAN_POINT('Ctrl Pts',(-40.9058333342005,-2.23615864849829,
-4.20560275094382));
#29615=CARTESIAN_POINT('Ctrl Pts',(-40.8793750008672,0.143960423897816,
-4.12248716145376));
#29616=CARTESIAN_POINT('Ctrl Pts',(-40.8529166675338,2.52407949629392,-4.03937157196371));
#29617=CARTESIAN_POINT('Ctrl Pts',(-40.8264583342005,3.64215882054307,-1.9365701964918));
#29618=CARTESIAN_POINT('Ctrl Pts',(-40.8000000008672,4.76023814479221,0.166231178980113));
#29619=CARTESIAN_POINT('Ctrl Pts',(-40.7735416675338,3.49819839664525,2.18591696496197));
#29620=CARTESIAN_POINT('Ctrl Pts',(-40.7470833342005,2.23615864849829,4.20560275094382));
#29621=CARTESIAN_POINT('Ctrl Pts',(-40.7206250008672,-0.143960423897816,
4.12248716145376));
#29622=CARTESIAN_POINT('Ctrl Pts',(-40.6941666675338,-2.52407949629392,
4.03937157196371));
#29623=CARTESIAN_POINT('Ctrl Pts',(-40.6677083342005,-3.64215882054307,
1.9365701964918));
#29624=CARTESIAN_POINT('Ctrl Pts',(-40.6412500008672,-4.76023814479221,
-0.166231178980113));
#29625=CARTESIAN_POINT('Ctrl Pts',(-40.6147916675338,-3.49819839664525,
-2.18591696496196));
#29626=CARTESIAN_POINT('Ctrl Pts',(-40.5883333342005,-2.23615864849829,
-4.20560275094382));
#29627=CARTESIAN_POINT('Ctrl Pts',(-40.5618750008672,0.143960423897816,
-4.12248716145376));
#29628=CARTESIAN_POINT('Ctrl Pts',(-40.5354166675338,2.52407949629392,-4.03937157196371));
#29629=CARTESIAN_POINT('Ctrl Pts',(-40.5089583342005,3.64215882054307,-1.9365701964918));
#29630=CARTESIAN_POINT('Ctrl Pts',(-40.4825000008672,4.76023814479221,0.166231178980113));
#29631=CARTESIAN_POINT('Ctrl Pts',(-40.4560416675338,3.49819839664525,2.18591696496197));
#29632=CARTESIAN_POINT('Ctrl Pts',(-40.4295833342005,2.23615864849829,4.20560275094382));
#29633=CARTESIAN_POINT('Ctrl Pts',(-40.4031250008672,-0.143960423897816,
4.12248716145376));
#29634=CARTESIAN_POINT('Ctrl Pts',(-40.3766666675338,-2.52407949629392,
4.03937157196371));
#29635=CARTESIAN_POINT('Ctrl Pts',(-40.3502083342005,-3.64215882054307,
1.9365701964918));
#29636=CARTESIAN_POINT('Ctrl Pts',(-40.3237500008672,-4.76023814479221,
-0.166231178980113));
#29637=CARTESIAN_POINT('Ctrl Pts',(-40.2972916675338,-3.49819839664525,
-2.18591696496196));
#29638=CARTESIAN_POINT('Ctrl Pts',(-40.2708333342005,-2.23615864849829,
-4.20560275094382));
#29639=CARTESIAN_POINT('Ctrl Pts',(-40.2443750008672,0.143960423897816,
-4.12248716145376));
#29640=CARTESIAN_POINT('Ctrl Pts',(-40.2179166675338,2.52407949629392,-4.03937157196371));
#29641=CARTESIAN_POINT('Ctrl Pts',(-40.1914583342005,3.64215882054307,-1.9365701964918));
#29642=CARTESIAN_POINT('Ctrl Pts',(-40.1650000008672,4.76023814479221,0.166231178980113));
#29643=CARTESIAN_POINT('Ctrl Pts',(-40.1385416675338,3.49819839664525,2.18591696496197));
#29644=CARTESIAN_POINT('Ctrl Pts',(-40.1120833342005,2.23615864849829,4.20560275094382));
#29645=CARTESIAN_POINT('Ctrl Pts',(-40.0856250008672,-0.143960423897816,
4.12248716145376));
#29646=CARTESIAN_POINT('Ctrl Pts',(-40.0591666675338,-2.52407949629392,
4.03937157196371));
#29647=CARTESIAN_POINT('Ctrl Pts',(-40.0327083342005,-3.64215882054307,
1.9365701964918));
#29648=CARTESIAN_POINT('Ctrl Pts',(-40.0062500008672,-4.76023814479221,
-0.166231178980113));
#29649=CARTESIAN_POINT('Ctrl Pts',(-39.9797916675338,-3.49819839664525,
-2.18591696496196));
#29650=CARTESIAN_POINT('Ctrl Pts',(-39.9533333342005,-2.23615864849829,
-4.20560275094382));
#29651=CARTESIAN_POINT('Ctrl Pts',(-39.9268750008672,0.143960423897816,
-4.12248716145376));
#29652=CARTESIAN_POINT('Ctrl Pts',(-39.9004166675338,2.52407949629392,-4.03937157196371));
#29653=CARTESIAN_POINT('Ctrl Pts',(-39.8739583342005,3.64215882054307,-1.9365701964918));
#29654=CARTESIAN_POINT('Ctrl Pts',(-39.8475000008672,4.76023814479221,0.166231178980113));
#29655=CARTESIAN_POINT('Ctrl Pts',(-39.8210416675338,3.49819839664525,2.18591696496197));
#29656=CARTESIAN_POINT('Ctrl Pts',(-39.7945833342005,2.23615864849829,4.20560275094382));
#29657=CARTESIAN_POINT('Ctrl Pts',(-39.7681250008672,-0.143960423897816,
4.12248716145376));
#29658=CARTESIAN_POINT('Ctrl Pts',(-39.7416666675338,-2.52407949629392,
4.03937157196371));
#29659=CARTESIAN_POINT('Ctrl Pts',(-39.7152083342005,-3.64215882054307,
1.9365701964918));
#29660=CARTESIAN_POINT('Ctrl Pts',(-39.6887500008672,-4.76023814479221,
-0.166231178980113));
#29661=CARTESIAN_POINT('Ctrl Pts',(-39.6622916675338,-3.49819839664525,
-2.18591696496196));
#29662=CARTESIAN_POINT('Ctrl Pts',(-39.6358333342005,-2.23615864849829,
-4.20560275094382));
#29663=CARTESIAN_POINT('Ctrl Pts',(-39.6093750008672,0.143960423897816,
-4.12248716145376));
#29664=CARTESIAN_POINT('Ctrl Pts',(-39.5829166675338,2.52407949629392,-4.03937157196371));
#29665=CARTESIAN_POINT('Ctrl Pts',(-39.5564583342005,3.64215882054307,-1.9365701964918));
#29666=CARTESIAN_POINT('Ctrl Pts',(-39.5300000008672,4.76023814479221,0.166231178980113));
#29667=CARTESIAN_POINT('Ctrl Pts',(-39.5035416675338,3.49819839664525,2.18591696496197));
#29668=CARTESIAN_POINT('Ctrl Pts',(-39.4770833342005,2.23615864849829,4.20560275094382));
#29669=CARTESIAN_POINT('Ctrl Pts',(-39.4506250008672,-0.143960423897816,
4.12248716145376));
#29670=CARTESIAN_POINT('Ctrl Pts',(-39.4241666675338,-2.52407949629392,
4.03937157196371));
#29671=CARTESIAN_POINT('Ctrl Pts',(-39.3977083342005,-3.64215882054307,
1.9365701964918));
#29672=CARTESIAN_POINT('Ctrl Pts',(-39.3712500008672,-4.76023814479221,
-0.166231178980113));
#29673=CARTESIAN_POINT('Ctrl Pts',(-39.3447916675338,-3.49819839664525,
-2.18591696496196));
#29674=CARTESIAN_POINT('Ctrl Pts',(-39.3183333342005,-2.23615864849829,
-4.20560275094382));
#29675=CARTESIAN_POINT('Ctrl Pts',(-39.2918750008672,0.143960423897816,
-4.12248716145376));
#29676=CARTESIAN_POINT('Ctrl Pts',(-39.2654166675338,2.52407949629392,-4.03937157196371));
#29677=CARTESIAN_POINT('Ctrl Pts',(-39.2389583342005,3.64215882054307,-1.9365701964918));
#29678=CARTESIAN_POINT('Ctrl Pts',(-39.2125000008672,4.76023814479221,0.166231178980113));
#29679=CARTESIAN_POINT('Ctrl Pts',(-39.1860416675338,3.49819839664525,2.18591696496197));
#29680=CARTESIAN_POINT('Ctrl Pts',(-39.1595833342005,2.23615864849829,4.20560275094382));
#29681=CARTESIAN_POINT('Ctrl Pts',(-39.1331250008672,-0.143960423897816,
4.12248716145376));
#29682=CARTESIAN_POINT('Ctrl Pts',(-39.1066666675338,-2.52407949629392,
4.03937157196371));
#29683=CARTESIAN_POINT('Ctrl Pts',(-39.0802083342005,-3.64215882054307,
1.9365701964918));
#29684=CARTESIAN_POINT('Ctrl Pts',(-39.0537500008672,-4.76023814479221,
-0.166231178980113));
#29685=CARTESIAN_POINT('Ctrl Pts',(-39.0272916675338,-3.49819839664525,
-2.18591696496196));
#29686=CARTESIAN_POINT('Ctrl Pts',(-39.0008333342005,-2.23615864849829,
-4.20560275094382));
#29687=CARTESIAN_POINT('Ctrl Pts',(-38.9743750008672,0.143960423897816,
-4.12248716145376));
#29688=CARTESIAN_POINT('Ctrl Pts',(-38.9479166675338,2.52407949629392,-4.03937157196371));
#29689=CARTESIAN_POINT('Ctrl Pts',(-38.9214583342005,3.64215882054307,-1.9365701964918));
#29690=CARTESIAN_POINT('Ctrl Pts',(-38.8950000008672,4.76023814479221,0.166231178980113));
#29691=CARTESIAN_POINT('Ctrl Pts',(-38.8685416675338,3.49819839664525,2.18591696496197));
#29692=CARTESIAN_POINT('Ctrl Pts',(-38.8420833342005,2.23615864849829,4.20560275094382));
#29693=CARTESIAN_POINT('Ctrl Pts',(-38.8156250008672,-0.143960423897816,
4.12248716145376));
#29694=CARTESIAN_POINT('Ctrl Pts',(-38.7891666675338,-2.52407949629392,
4.03937157196371));
#29695=CARTESIAN_POINT('Ctrl Pts',(-38.7627083342005,-3.64215882054307,
1.9365701964918));
#29696=CARTESIAN_POINT('Ctrl Pts',(-38.7362500008672,-4.76023814479221,
-0.166231178980113));
#29697=CARTESIAN_POINT('Ctrl Pts',(-38.7097916675338,-3.49819839664525,
-2.18591696496196));
#29698=CARTESIAN_POINT('Ctrl Pts',(-38.6833333342005,-2.23615864849829,
-4.20560275094382));
#29699=CARTESIAN_POINT('Ctrl Pts',(-38.6568750008672,0.143960423897816,
-4.12248716145376));
#29700=CARTESIAN_POINT('Ctrl Pts',(-38.6304166675338,2.52407949629392,-4.03937157196371));
#29701=CARTESIAN_POINT('Ctrl Pts',(-38.6039583342005,3.64215882054307,-1.9365701964918));
#29702=CARTESIAN_POINT('Ctrl Pts',(-38.5775000008672,4.76023814479221,0.166231178980113));
#29703=CARTESIAN_POINT('Ctrl Pts',(-38.5510416675338,3.49819839664525,2.18591696496197));
#29704=CARTESIAN_POINT('Ctrl Pts',(-38.5245833342005,2.23615864849829,4.20560275094382));
#29705=CARTESIAN_POINT('Ctrl Pts',(-38.4981250008672,-0.143960423897816,
4.12248716145376));
#29706=CARTESIAN_POINT('Ctrl Pts',(-38.4716666675338,-2.52407949629392,
4.03937157196371));
#29707=CARTESIAN_POINT('Ctrl Pts',(-38.4452083342005,-3.64215882054307,
1.9365701964918));
#29708=CARTESIAN_POINT('Ctrl Pts',(-38.4187500008672,-4.76023814479221,
-0.166231178980113));
#29709=CARTESIAN_POINT('Ctrl Pts',(-38.3922916675338,-3.49819839664525,
-2.18591696496196));
#29710=CARTESIAN_POINT('Ctrl Pts',(-38.3658333342005,-2.23615864849829,
-4.20560275094382));
#29711=CARTESIAN_POINT('Ctrl Pts',(-38.3393750008672,0.143960423897816,
-4.12248716145376));
#29712=CARTESIAN_POINT('Ctrl Pts',(-38.3129166675338,2.52407949629392,-4.03937157196371));
#29713=CARTESIAN_POINT('Ctrl Pts',(-38.2864583342005,3.64215882054307,-1.9365701964918));
#29714=CARTESIAN_POINT('Ctrl Pts',(-38.2600000008672,4.76023814479221,0.166231178980113));
#29715=CARTESIAN_POINT('Ctrl Pts',(-38.2335416675338,3.49819839664525,2.18591696496197));
#29716=CARTESIAN_POINT('Ctrl Pts',(-38.2070833342005,2.23615864849829,4.20560275094382));
#29717=CARTESIAN_POINT('Ctrl Pts',(-38.1806250008672,-0.143960423897816,
4.12248716145376));
#29718=CARTESIAN_POINT('Ctrl Pts',(-38.1541666675338,-2.52407949629392,
4.03937157196371));
#29719=CARTESIAN_POINT('Ctrl Pts',(-38.1277083342005,-3.64215882054307,
1.9365701964918));
#29720=CARTESIAN_POINT('Ctrl Pts',(-38.1012500008672,-4.76023814479221,
-0.166231178980113));
#29721=CARTESIAN_POINT('Ctrl Pts',(-38.0747916675338,-3.49819839664525,
-2.18591696496196));
#29722=CARTESIAN_POINT('Ctrl Pts',(-38.0483333342005,-2.23615864849829,
-4.20560275094382));
#29723=CARTESIAN_POINT('Ctrl Pts',(-38.0218750008672,0.143960423897816,
-4.12248716145376));
#29724=CARTESIAN_POINT('Ctrl Pts',(-37.9954166675338,2.52407949629392,-4.03937157196371));
#29725=CARTESIAN_POINT('Ctrl Pts',(-37.9689583342005,3.64215882054307,-1.9365701964918));
#29726=CARTESIAN_POINT('Ctrl Pts',(-37.9425000008672,4.76023814479221,0.166231178980113));
#29727=CARTESIAN_POINT('Ctrl Pts',(-37.9160416675338,3.49819839664525,2.18591696496197));
#29728=CARTESIAN_POINT('Ctrl Pts',(-37.8895833342005,2.23615864849829,4.20560275094382));
#29729=CARTESIAN_POINT('Ctrl Pts',(-37.8631250008672,-0.143960423897816,
4.12248716145376));
#29730=CARTESIAN_POINT('Ctrl Pts',(-37.8366666675338,-2.52407949629392,
4.03937157196371));
#29731=CARTESIAN_POINT('Ctrl Pts',(-37.8102083342005,-3.64215882054307,
1.9365701964918));
#29732=CARTESIAN_POINT('Ctrl Pts',(-37.7837500008672,-4.76023814479221,
-0.166231178980113));
#29733=CARTESIAN_POINT('Ctrl Pts',(-37.7572916675338,-3.49819839664525,
-2.18591696496196));
#29734=CARTESIAN_POINT('Ctrl Pts',(-37.7308333342005,-2.23615864849829,
-4.20560275094382));
#29735=CARTESIAN_POINT('Ctrl Pts',(-37.7043750008672,0.143960423897816,
-4.12248716145376));
#29736=CARTESIAN_POINT('Ctrl Pts',(-37.6779166675338,2.52407949629392,-4.03937157196371));
#29737=CARTESIAN_POINT('Ctrl Pts',(-37.6514583342005,3.64215882054307,-1.9365701964918));
#29738=CARTESIAN_POINT('Ctrl Pts',(-37.6250000008672,4.76023814479221,0.166231178980113));
#29739=CARTESIAN_POINT('Ctrl Pts',(-37.5985416675338,3.49819839664525,2.18591696496197));
#29740=CARTESIAN_POINT('Ctrl Pts',(-37.5720833342005,2.23615864849829,4.20560275094382));
#29741=CARTESIAN_POINT('Ctrl Pts',(-37.5456250008672,-0.143960423897816,
4.12248716145376));
#29742=CARTESIAN_POINT('Ctrl Pts',(-37.5191666675338,-2.52407949629392,
4.03937157196371));
#29743=CARTESIAN_POINT('Ctrl Pts',(-37.4927083342005,-3.64215882054307,
1.9365701964918));
#29744=CARTESIAN_POINT('Ctrl Pts',(-37.4662500008672,-4.76023814479221,
-0.166231178980113));
#29745=CARTESIAN_POINT('Ctrl Pts',(-37.4397916675338,-3.49819839664525,
-2.18591696496196));
#29746=CARTESIAN_POINT('Ctrl Pts',(-37.4133333342005,-2.23615864849829,
-4.20560275094382));
#29747=CARTESIAN_POINT('Ctrl Pts',(-37.3868750008672,0.143960423897816,
-4.12248716145376));
#29748=CARTESIAN_POINT('Ctrl Pts',(-37.3604166675338,2.52407949629392,-4.03937157196371));
#29749=CARTESIAN_POINT('Ctrl Pts',(-37.3339583342005,3.64215882054307,-1.9365701964918));
#29750=CARTESIAN_POINT('Ctrl Pts',(-37.3075000008672,4.76023814479221,0.166231178980113));
#29751=CARTESIAN_POINT('Ctrl Pts',(-37.2810416675338,3.49819839664525,2.18591696496197));
#29752=CARTESIAN_POINT('Ctrl Pts',(-37.2545833342005,2.23615864849829,4.20560275094382));
#29753=CARTESIAN_POINT('Ctrl Pts',(-37.2281250008672,-0.143960423897816,
4.12248716145376));
#29754=CARTESIAN_POINT('Ctrl Pts',(-37.2016666675338,-2.52407949629392,
4.03937157196371));
#29755=CARTESIAN_POINT('Ctrl Pts',(-37.1752083342005,-3.64215882054307,
1.9365701964918));
#29756=CARTESIAN_POINT('Ctrl Pts',(-37.1487500008672,-4.76023814479221,
-0.166231178980113));
#29757=CARTESIAN_POINT('Ctrl Pts',(-37.1222916675338,-3.49819839664525,
-2.18591696496196));
#29758=CARTESIAN_POINT('Ctrl Pts',(-37.0958333342005,-2.23615864849829,
-4.20560275094382));
#29759=CARTESIAN_POINT('Ctrl Pts',(-37.0693750008672,0.143960423897816,
-4.12248716145376));
#29760=CARTESIAN_POINT('Ctrl Pts',(-37.0429166675338,2.52407949629392,-4.03937157196371));
#29761=CARTESIAN_POINT('Ctrl Pts',(-37.0164583342005,3.64215882054307,-1.9365701964918));
#29762=CARTESIAN_POINT('Ctrl Pts',(-36.9900000008672,4.76023814479221,0.166231178980113));
#29763=CARTESIAN_POINT('Ctrl Pts',(-36.9635416675338,3.49819839664525,2.18591696496197));
#29764=CARTESIAN_POINT('Ctrl Pts',(-36.9370833342005,2.23615864849829,4.20560275094382));
#29765=CARTESIAN_POINT('Ctrl Pts',(-36.9106250008672,-0.143960423897816,
4.12248716145376));
#29766=CARTESIAN_POINT('Ctrl Pts',(-36.8841666675338,-2.52407949629392,
4.03937157196371));
#29767=CARTESIAN_POINT('Ctrl Pts',(-36.8577083342005,-3.64215882054307,
1.9365701964918));
#29768=CARTESIAN_POINT('Ctrl Pts',(-36.8312500008672,-4.76023814479221,
-0.166231178980113));
#29769=CARTESIAN_POINT('Ctrl Pts',(-36.8047916675338,-3.49819839664525,
-2.18591696496196));
#29770=CARTESIAN_POINT('Ctrl Pts',(-36.7783333342005,-2.23615864849829,
-4.20560275094382));
#29771=CARTESIAN_POINT('Ctrl Pts',(-36.7518750008672,0.143960423897816,
-4.12248716145376));
#29772=CARTESIAN_POINT('Ctrl Pts',(-36.7254166675338,2.52407949629392,-4.03937157196371));
#29773=CARTESIAN_POINT('Ctrl Pts',(-36.6989583342005,3.64215882054307,-1.9365701964918));
#29774=CARTESIAN_POINT('Ctrl Pts',(-36.6725000008672,4.76023814479221,0.166231178980113));
#29775=CARTESIAN_POINT('Ctrl Pts',(-36.6460416675338,3.49819839664525,2.18591696496197));
#29776=CARTESIAN_POINT('Ctrl Pts',(-36.6195833342005,2.23615864849829,4.20560275094382));
#29777=CARTESIAN_POINT('Ctrl Pts',(-36.5931250008672,-0.143960423897816,
4.12248716145376));
#29778=CARTESIAN_POINT('Ctrl Pts',(-36.5666666675338,-2.52407949629392,
4.03937157196371));
#29779=CARTESIAN_POINT('Ctrl Pts',(-36.5402083342005,-3.64215882054307,
1.9365701964918));
#29780=CARTESIAN_POINT('Ctrl Pts',(-36.5137500008672,-4.76023814479221,
-0.166231178980113));
#29781=CARTESIAN_POINT('Ctrl Pts',(-36.4872916675338,-3.49819839664525,
-2.18591696496196));
#29782=CARTESIAN_POINT('Ctrl Pts',(-36.4608333342005,-2.23615864849829,
-4.20560275094382));
#29783=CARTESIAN_POINT('Ctrl Pts',(-36.4343750008672,0.143960423897816,
-4.12248716145376));
#29784=CARTESIAN_POINT('Ctrl Pts',(-36.4079166675338,2.52407949629392,-4.03937157196371));
#29785=CARTESIAN_POINT('Ctrl Pts',(-36.3814583342005,3.64215882054307,-1.9365701964918));
#29786=CARTESIAN_POINT('Ctrl Pts',(-36.3550000008672,4.76023814479221,0.166231178980113));
#29787=CARTESIAN_POINT('Ctrl Pts',(-36.3285416675338,3.49819839664525,2.18591696496197));
#29788=CARTESIAN_POINT('Ctrl Pts',(-36.3020833342005,2.23615864849829,4.20560275094382));
#29789=CARTESIAN_POINT('Ctrl Pts',(-36.2756250008672,-0.143960423897816,
4.12248716145376));
#29790=CARTESIAN_POINT('Ctrl Pts',(-36.2491666675338,-2.52407949629392,
4.03937157196371));
#29791=CARTESIAN_POINT('Ctrl Pts',(-36.2227083342005,-3.64215882054307,
1.9365701964918));
#29792=CARTESIAN_POINT('Ctrl Pts',(-36.1962500008672,-4.76023814479221,
-0.166231178980113));
#29793=CARTESIAN_POINT('Ctrl Pts',(-36.1697916675338,-3.49819839664525,
-2.18591696496196));
#29794=CARTESIAN_POINT('Ctrl Pts',(-36.1433333342005,-2.23615864849829,
-4.20560275094382));
#29795=CARTESIAN_POINT('Ctrl Pts',(-36.1168750008672,0.143960423897816,
-4.12248716145376));
#29796=CARTESIAN_POINT('Ctrl Pts',(-36.0904166675338,2.52407949629392,-4.03937157196371));
#29797=CARTESIAN_POINT('Ctrl Pts',(-36.0639583342005,3.64215882054307,-1.9365701964918));
#29798=CARTESIAN_POINT('Ctrl Pts',(-36.0375000008672,4.76023814479221,0.166231178980113));
#29799=CARTESIAN_POINT('Ctrl Pts',(-36.0110416675338,3.49819839664525,2.18591696496197));
#29800=CARTESIAN_POINT('Ctrl Pts',(-35.9845833342005,2.23615864849829,4.20560275094382));
#29801=CARTESIAN_POINT('Ctrl Pts',(-35.9581250008672,-0.143960423897816,
4.12248716145376));
#29802=CARTESIAN_POINT('Ctrl Pts',(-35.9316666675338,-2.52407949629392,
4.03937157196371));
#29803=CARTESIAN_POINT('Ctrl Pts',(-35.9052083342005,-3.64215882054307,
1.9365701964918));
#29804=CARTESIAN_POINT('Ctrl Pts',(-35.8787500008672,-4.76023814479221,
-0.166231178980113));
#29805=CARTESIAN_POINT('Ctrl Pts',(-35.8522916675338,-3.49819839664525,
-2.18591696496196));
#29806=CARTESIAN_POINT('Ctrl Pts',(-35.8258333342005,-2.23615864849829,
-4.20560275094382));
#29807=CARTESIAN_POINT('Ctrl Pts',(-35.7993750008672,0.143960423897816,
-4.12248716145376));
#29808=CARTESIAN_POINT('Ctrl Pts',(-35.7729166675338,2.52407949629392,-4.03937157196371));
#29809=CARTESIAN_POINT('Ctrl Pts',(-35.7464583342005,3.64215882054307,-1.9365701964918));
#29810=CARTESIAN_POINT('Ctrl Pts',(-35.7200000008672,4.76023814479221,0.166231178980113));
#29811=CARTESIAN_POINT('Ctrl Pts',(-35.6935416675338,3.49819839664525,2.18591696496197));
#29812=CARTESIAN_POINT('Ctrl Pts',(-35.6670833342005,2.23615864849829,4.20560275094382));
#29813=CARTESIAN_POINT('Ctrl Pts',(-35.6406250008672,-0.143960423897816,
4.12248716145376));
#29814=CARTESIAN_POINT('Ctrl Pts',(-35.6141666675338,-2.52407949629392,
4.03937157196371));
#29815=CARTESIAN_POINT('Ctrl Pts',(-35.5877083342005,-3.64215882054307,
1.9365701964918));
#29816=CARTESIAN_POINT('Ctrl Pts',(-35.5612500008672,-4.76023814479221,
-0.166231178980113));
#29817=CARTESIAN_POINT('Ctrl Pts',(-35.5347916675338,-3.49819839664525,
-2.18591696496196));
#29818=CARTESIAN_POINT('Ctrl Pts',(-35.5083333342005,-2.23615864849829,
-4.20560275094382));
#29819=CARTESIAN_POINT('Ctrl Pts',(-35.4818750008672,0.143960423897816,
-4.12248716145376));
#29820=CARTESIAN_POINT('Ctrl Pts',(-35.4554166675338,2.52407949629392,-4.03937157196371));
#29821=CARTESIAN_POINT('Ctrl Pts',(-35.4289583342005,3.64215882054307,-1.9365701964918));
#29822=CARTESIAN_POINT('Ctrl Pts',(-35.4025000008672,4.76023814479221,0.166231178980113));
#29823=CARTESIAN_POINT('Ctrl Pts',(-35.3760416675338,3.49819839664525,2.18591696496197));
#29824=CARTESIAN_POINT('Ctrl Pts',(-35.3495833342005,2.23615864849829,4.20560275094382));
#29825=CARTESIAN_POINT('Ctrl Pts',(-35.3231250008672,-0.143960423897816,
4.12248716145376));
#29826=CARTESIAN_POINT('Ctrl Pts',(-35.2966666675338,-2.52407949629392,
4.03937157196371));
#29827=CARTESIAN_POINT('Ctrl Pts',(-35.2702083342005,-3.64215882054307,
1.9365701964918));
#29828=CARTESIAN_POINT('Ctrl Pts',(-35.2437500008672,-4.76023814479221,
-0.166231178980113));
#29829=CARTESIAN_POINT('Ctrl Pts',(-35.2172916675338,-3.49819839664525,
-2.18591696496196));
#29830=CARTESIAN_POINT('Ctrl Pts',(-35.1908333342005,-2.23615864849829,
-4.20560275094382));
#29831=CARTESIAN_POINT('Ctrl Pts',(-35.1643750008672,0.143960423897816,
-4.12248716145376));
#29832=CARTESIAN_POINT('Ctrl Pts',(-35.1379166675338,2.52407949629392,-4.03937157196371));
#29833=CARTESIAN_POINT('Ctrl Pts',(-35.1114583342005,3.64215882054307,-1.9365701964918));
#29834=CARTESIAN_POINT('Ctrl Pts',(-35.0850000008672,4.76023814479221,0.166231178980113));
#29835=CARTESIAN_POINT('Ctrl Pts',(-35.0585416675338,3.49819839664525,2.18591696496197));
#29836=CARTESIAN_POINT('Ctrl Pts',(-35.0320833342005,2.23615864849829,4.20560275094382));
#29837=CARTESIAN_POINT('Ctrl Pts',(-35.0056250008672,-0.143960423897816,
4.12248716145376));
#29838=CARTESIAN_POINT('Ctrl Pts',(-34.9791666675338,-2.52407949629392,
4.03937157196371));
#29839=CARTESIAN_POINT('Ctrl Pts',(-34.9527083342005,-3.64215882054307,
1.9365701964918));
#29840=CARTESIAN_POINT('Ctrl Pts',(-34.9262500008672,-4.76023814479221,
-0.166231178980113));
#29841=CARTESIAN_POINT('Ctrl Pts',(-34.8997916675338,-3.49819839664525,
-2.18591696496196));
#29842=CARTESIAN_POINT('Ctrl Pts',(-34.8733333342005,-2.23615864849829,
-4.20560275094382));
#29843=CARTESIAN_POINT('Ctrl Pts',(-34.8468750008672,0.143960423897816,
-4.12248716145376));
#29844=CARTESIAN_POINT('Ctrl Pts',(-34.8204166675338,2.52407949629392,-4.03937157196371));
#29845=CARTESIAN_POINT('Ctrl Pts',(-34.7939583342005,3.64215882054307,-1.9365701964918));
#29846=CARTESIAN_POINT('Ctrl Pts',(-34.7675000008672,4.76023814479221,0.166231178980113));
#29847=CARTESIAN_POINT('Ctrl Pts',(-34.7410416675338,3.49819839664525,2.18591696496197));
#29848=CARTESIAN_POINT('Ctrl Pts',(-34.7145833342005,2.23615864849829,4.20560275094382));
#29849=CARTESIAN_POINT('Ctrl Pts',(-34.6881250008672,-0.143960423897816,
4.12248716145376));
#29850=CARTESIAN_POINT('Ctrl Pts',(-34.6616666675338,-2.52407949629392,
4.03937157196371));
#29851=CARTESIAN_POINT('Ctrl Pts',(-34.6352083342005,-3.64215882054307,
1.9365701964918));
#29852=CARTESIAN_POINT('Ctrl Pts',(-34.6087500008672,-4.76023814479221,
-0.166231178980113));
#29853=CARTESIAN_POINT('Ctrl Pts',(-34.5822916675338,-3.49819839664525,
-2.18591696496196));
#29854=CARTESIAN_POINT('Ctrl Pts',(-34.5558333342005,-2.23615864849829,
-4.20560275094382));
#29855=CARTESIAN_POINT('Ctrl Pts',(-34.5293750008672,0.143960423897816,
-4.12248716145376));
#29856=CARTESIAN_POINT('Ctrl Pts',(-34.5029166675338,2.52407949629392,-4.03937157196371));
#29857=CARTESIAN_POINT('Ctrl Pts',(-34.4764583342005,3.64215882054307,-1.9365701964918));
#29858=CARTESIAN_POINT('Ctrl Pts',(-34.4500000008672,4.76023814479221,0.166231178980113));
#29859=CARTESIAN_POINT('Ctrl Pts',(-34.4235416675338,3.49819839664525,2.18591696496197));
#29860=CARTESIAN_POINT('Ctrl Pts',(-34.3970833342005,2.23615864849829,4.20560275094382));
#29861=CARTESIAN_POINT('Ctrl Pts',(-34.3706250008672,-0.143960423897816,
4.12248716145376));
#29862=CARTESIAN_POINT('Ctrl Pts',(-34.3441666675338,-2.52407949629392,
4.03937157196371));
#29863=CARTESIAN_POINT('Ctrl Pts',(-34.3177083342005,-3.64215882054307,
1.9365701964918));
#29864=CARTESIAN_POINT('Ctrl Pts',(-34.2912500008672,-4.76023814479221,
-0.166231178980113));
#29865=CARTESIAN_POINT('Ctrl Pts',(-34.2647916675338,-3.49819839664525,
-2.18591696496196));
#29866=CARTESIAN_POINT('Ctrl Pts',(-34.2383333342005,-2.23615864849829,
-4.20560275094382));
#29867=CARTESIAN_POINT('Ctrl Pts',(-34.2118750008672,0.143960423897816,
-4.12248716145376));
#29868=CARTESIAN_POINT('Ctrl Pts',(-34.1854166675338,2.52407949629392,-4.03937157196371));
#29869=CARTESIAN_POINT('Ctrl Pts',(-34.1589583342005,3.64215882054307,-1.9365701964918));
#29870=CARTESIAN_POINT('Ctrl Pts',(-34.1325000008672,4.76023814479221,0.166231178980113));
#29871=CARTESIAN_POINT('Ctrl Pts',(-34.1060416675338,3.49819839664525,2.18591696496197));
#29872=CARTESIAN_POINT('Ctrl Pts',(-34.0795833342005,2.23615864849829,4.20560275094382));
#29873=CARTESIAN_POINT('Ctrl Pts',(-34.0531250008672,-0.143960423897816,
4.12248716145376));
#29874=CARTESIAN_POINT('Ctrl Pts',(-34.0266666675338,-2.52407949629392,
4.03937157196371));
#29875=CARTESIAN_POINT('Ctrl Pts',(-34.0002083342005,-3.64215882054307,
1.9365701964918));
#29876=CARTESIAN_POINT('Ctrl Pts',(-33.9737500008672,-4.76023814479221,
-0.166231178980113));
#29877=CARTESIAN_POINT('Ctrl Pts',(-33.9472916675338,-3.49819839664525,
-2.18591696496196));
#29878=CARTESIAN_POINT('Ctrl Pts',(-33.9208333342005,-2.23615864849829,
-4.20560275094382));
#29879=CARTESIAN_POINT('Ctrl Pts',(-33.8943750008672,0.143960423897816,
-4.12248716145376));
#29880=CARTESIAN_POINT('Ctrl Pts',(-33.8679166675338,2.52407949629392,-4.03937157196371));
#29881=CARTESIAN_POINT('Ctrl Pts',(-33.8414583342005,3.64215882054307,-1.9365701964918));
#29882=CARTESIAN_POINT('Ctrl Pts',(-33.8150000008672,4.76023814479221,0.166231178980113));
#29883=CARTESIAN_POINT('Ctrl Pts',(-33.7885416675338,3.49819839664525,2.18591696496197));
#29884=CARTESIAN_POINT('Ctrl Pts',(-33.7628337716481,2.27195386943706,4.14831842290086));
#29885=CARTESIAN_POINT('Ctrl Pts',(-33.73676661727,-0.0419478961855304,
4.12478670648623));
#29886=CARTESIAN_POINT('',(0.,0.,0.));
#29887=CARTESIAN_POINT('Origin',(0.,4.,0.));
#29888=CARTESIAN_POINT('',(-9.85840673313619E-16,4.,8.05));
#29889=CARTESIAN_POINT('Origin',(0.,4.,0.));
#29890=CARTESIAN_POINT('',(-9.85840673313619E-16,2.,8.05));
#29891=CARTESIAN_POINT('',(-9.85840673313619E-16,4.,8.05));
#29892=CARTESIAN_POINT('Origin',(0.,2.,0.));
#29893=CARTESIAN_POINT('Origin',(0.,2.,0.));
#29894=CARTESIAN_POINT('',(-1.28587913910472E-15,0.,10.5));
#29895=CARTESIAN_POINT('Origin',(0.,0.,0.));
#29896=CARTESIAN_POINT('',(-1.28587913910472E-15,4.,10.5));
#29897=CARTESIAN_POINT('',(-1.28587913910472E-15,2.,10.5));
#29898=CARTESIAN_POINT('Origin',(0.,4.,0.));
#29899=CARTESIAN_POINT('Origin',(0.,0.,0.));
#29900=CARTESIAN_POINT('Origin',(0.,4.,0.));
#29901=CARTESIAN_POINT('Origin',(0.,2.,0.));
#29902=CARTESIAN_POINT('',(0.,0.,0.));
#29903=CARTESIAN_POINT('Origin',(0.,5.,0.));
#29904=CARTESIAN_POINT('',(-2.75545529808155E-15,5.,22.5));
#29905=CARTESIAN_POINT('Origin',(0.,5.,0.));
#29906=CARTESIAN_POINT('',(-2.75545529808155E-15,0.,22.5));
#29907=CARTESIAN_POINT('',(-2.75545529808155E-15,5.,22.5));
#29908=CARTESIAN_POINT('Origin',(0.,0.,0.));
#29909=CARTESIAN_POINT('Origin',(0.,5.,0.));
#29910=CARTESIAN_POINT('',(-3.06161699786838E-15,0.,25.));
#29911=CARTESIAN_POINT('Origin',(0.,0.,0.));
#29912=CARTESIAN_POINT('',(-3.06161699786838E-15,5.,25.));
#29913=CARTESIAN_POINT('',(-3.06161699786838E-15,5.,25.));
#29914=CARTESIAN_POINT('Origin',(0.,5.,0.));
#29915=CARTESIAN_POINT('Origin',(0.,5.,0.));
#29916=CARTESIAN_POINT('Origin',(0.,0.,0.));
#29917=CARTESIAN_POINT('',(0.,0.,0.));
#29918=CARTESIAN_POINT('Origin',(0.,0.,-0.5));
#29919=CARTESIAN_POINT('',(-3.,3.67394039744206E-16,-0.5));
#29920=CARTESIAN_POINT('',(3.,-3.67394039744206E-16,-0.5));
#29921=CARTESIAN_POINT('Origin',(0.,0.,-0.5));
#29922=CARTESIAN_POINT('Origin',(0.,0.,-0.5));
#29923=CARTESIAN_POINT('',(2.5,-3.06161699786838E-16,0.));
#29924=CARTESIAN_POINT('Origin',(2.5,-3.06161699786838E-16,-0.5));
#29925=CARTESIAN_POINT('Origin',(0.,0.,0.));
#29926=CARTESIAN_POINT('Origin',(0.,0.,-11.5));
#29927=CARTESIAN_POINT('',(-3.,-3.67394039744206E-16,-11.5));
#29928=CARTESIAN_POINT('Origin',(0.,0.,-11.5));
#29929=CARTESIAN_POINT('',(-2.5,-3.06161699786838E-16,-12.));
#29930=CARTESIAN_POINT('Origin',(-2.5,-3.06161699786838E-16,-11.5));
#29931=CARTESIAN_POINT('Origin',(0.,0.,-12.));
#29932=CARTESIAN_POINT('Origin',(0.,0.,0.));
#29933=CARTESIAN_POINT('',(-2.5,-3.06161699786838E-16,-22.));
#29934=CARTESIAN_POINT('',(-2.5,-3.06161699786838E-16,0.));
#29935=CARTESIAN_POINT('Origin',(0.,0.,-22.));
#29936=CARTESIAN_POINT('Origin',(0.,0.,0.));
#29937=CARTESIAN_POINT('',(-3.,-3.67394039744206E-16,0.));
#29938=CARTESIAN_POINT('Origin',(0.,0.,0.));
#29939=CARTESIAN_POINT('Origin',(0.,2.5,-22.));
#29940=CARTESIAN_POINT('',(0.,0.,0.));
#29941=CARTESIAN_POINT('Origin',(0.,0.,13.4833147735479));
#29942=CARTESIAN_POINT('',(8.,-9.79717439317882E-16,11.4833147735479));
#29943=CARTESIAN_POINT('Origin',(0.,0.,11.4833147735479));
#29944=CARTESIAN_POINT('',(10.,-1.22464679914735E-15,13.4833147735479));
#29945=CARTESIAN_POINT('Origin',(8.,-9.79717439317882E-16,13.4833147735479));
#29946=CARTESIAN_POINT('Origin',(0.,0.,13.4833147735479));
#29947=CARTESIAN_POINT('Origin',(0.,0.,0.));
#29948=CARTESIAN_POINT('',(10.,-1.22464679914735E-15,14.9833147735479));
#29949=CARTESIAN_POINT('',(10.,-1.22464679914735E-15,0.));
#29950=CARTESIAN_POINT('Origin',(0.,0.,14.9833147735479));
#29951=CARTESIAN_POINT('Origin',(0.,0.,14.9833147735479));
#29952=CARTESIAN_POINT('',(9.5,-1.16341445918999E-15,15.4833147735479));
#29953=CARTESIAN_POINT('',(10.,-1.22464679914735E-15,14.9833147735479));
#29954=CARTESIAN_POINT('Origin',(0.,0.,15.4833147735479));
#29955=CARTESIAN_POINT('Origin',(0.,0.,0.));
#29956=CARTESIAN_POINT('',(4.,-4.89858719658941E-16,15.4833147735479));
#29957=CARTESIAN_POINT('Origin',(0.,0.,15.4833147735479));
#29958=CARTESIAN_POINT('',(4.,-4.89858719658941E-16,22.9833147735479));
#29959=CARTESIAN_POINT('',(4.,-4.89858719658941E-16,0.));
#29960=CARTESIAN_POINT('Origin',(0.,0.,22.9833147735479));
#29961=CARTESIAN_POINT('Origin',(0.,0.,22.9833147735479));
#29962=CARTESIAN_POINT('',(3.5,-4.28626379701573E-16,23.4833147735479));
#29963=CARTESIAN_POINT('',(4.,-4.89858719658941E-16,22.9833147735479));
#29964=CARTESIAN_POINT('Origin',(0.,0.,23.4833147735479));
#29965=CARTESIAN_POINT('Origin',(0.,0.,0.));
#29966=CARTESIAN_POINT('',(9.,-5.51091059616309E-16,-6.74891902197836E-32));
#29967=CARTESIAN_POINT('',(-9.,-5.51091059616309E-16,-6.74891902197836E-32));
#29968=CARTESIAN_POINT('Origin',(0.,0.,0.));
#29969=CARTESIAN_POINT('',(5.,-6.12323399573676E-16,7.48331477354788));
#29970=CARTESIAN_POINT('Origin',(0.,0.,7.48331477354788));
#29971=CARTESIAN_POINT('Origin',(0.,0.,0.));
#29972=CARTESIAN_POINT('',(5.,-6.12323399573676E-16,11.4833147735479));
#29973=CARTESIAN_POINT('',(5.,-6.12323399573676E-16,0.));
#29974=CARTESIAN_POINT('Origin',(0.,0.,11.4833147735479));
#29975=CARTESIAN_POINT('Origin',(0.,5.,11.4833147735479));
#29976=CARTESIAN_POINT('Origin',(0.,3.5,23.4833147735479));
#29977=CARTESIAN_POINT('Origin',(0.,4.,15.4833147735479));
#29978=CARTESIAN_POINT('',(0.,0.,0.));
#29979=CARTESIAN_POINT('Origin',(-3.88784034431744,0.,0.));
#29980=CARTESIAN_POINT('',(-2.89487755360751,-1.11668521385931E-15,9.11842675485531));
#29981=CARTESIAN_POINT('Origin',(-2.89487755360751,0.,0.));
#29982=CARTESIAN_POINT('',(-3.88784034431744,-9.62148232812991E-16,7.85653654166145));
#29983=CARTESIAN_POINT('',(-3.88784034431744,-9.62148232812991E-16,7.85653654166145));
#29984=CARTESIAN_POINT('Origin',(-3.88784034431744,0.,0.));
#29985=CARTESIAN_POINT('Origin',(32.1691171325868,-6.,-3.60555127546399));
#29986=CARTESIAN_POINT('',(32.9519577972005,-6.53333333333333,-3.9260447221719));
#29987=CARTESIAN_POINT('',(32.1691171325868,-5.,-3.60555127546399));
#29988=CARTESIAN_POINT('Origin',(32.1691171325868,-6.,-3.60555127546399));
#29989=CARTESIAN_POINT('',(32.1691171325868,-5.14285714285715,-3.09047252182628));
#29990=CARTESIAN_POINT('Origin',(32.1691171325868,-6.,-3.60555127546399));
#29991=CARTESIAN_POINT('Origin',(32.1691171325868,-6.,-3.60555127546399));
#29992=CARTESIAN_POINT('Origin',(32.1691171325868,0.,0.));
#29993=CARTESIAN_POINT('',(32.1691171325868,5.14285714285714,-3.09047252182628));
#29994=CARTESIAN_POINT('Origin',(32.1691171325868,0.,0.));
#29995=CARTESIAN_POINT('',(32.9519577972005,6.53333333333333,-3.9260447221719));
#29996=CARTESIAN_POINT('Origin',(32.1691171325868,6.,-3.60555127546399));
#29997=CARTESIAN_POINT('Origin',(32.9519577972005,0.,0.));
#29998=CARTESIAN_POINT('Origin',(-60.4312629272455,0.,0.));
#29999=CARTESIAN_POINT('',(31.6603850692973,-5.1428571428572,-3.09047252182618));
#30000=CARTESIAN_POINT('',(-60.4312629272455,-5.1428571428572,-3.09047252182618));
#30001=CARTESIAN_POINT('',(31.2718056654608,-5.57521816165486,-2.21741796916002));
#30002=CARTESIAN_POINT('Ctrl Pts',(31.6603850692973,-5.1428571428572,-3.09047252182618));
#30003=CARTESIAN_POINT('Ctrl Pts',(31.6130789304298,-5.19901889001868,-2.99701372531371));
#30004=CARTESIAN_POINT('Ctrl Pts',(31.566662826541,-5.25269307059619,-2.90193250281435));
#30005=CARTESIAN_POINT('Ctrl Pts',(31.5214090737152,-5.30390019323349,-2.80511011195956));
#30006=CARTESIAN_POINT('Ctrl Pts',(31.4766400999664,-5.35455876154984,-2.70932492722243));
#30007=CARTESIAN_POINT('Ctrl Pts',(31.4330087073867,-5.40280302228635,-2.61183520986889));
#30008=CARTESIAN_POINT('Ctrl Pts',(31.3907785539495,-5.4486054329858,-2.51250847473946));
#30009=CARTESIAN_POINT('Ctrl Pts',(31.3497152496182,-5.49314229057631,-2.41592620778376));
#30010=CARTESIAN_POINT('Ctrl Pts',(31.3099768197504,-5.53537039074759,-2.3176065755272));
#30011=CARTESIAN_POINT('Ctrl Pts',(31.2718056654607,-5.57521816165486,-2.21741796916003));
#30012=CARTESIAN_POINT('',(31.2718056654608,5.57521816165486,-2.21741796916003));
#30013=CARTESIAN_POINT('Origin',(31.2718056654608,0.,0.));
#30014=CARTESIAN_POINT('',(31.6603850692973,5.14285714285714,-3.09047252182628));
#30015=CARTESIAN_POINT('Ctrl Pts',(31.2718056654607,5.57521816165486,-2.21741796916003));
#30016=CARTESIAN_POINT('Ctrl Pts',(31.3109482377269,5.53435630454291,-2.32015627608185));
#30017=CARTESIAN_POINT('Ctrl Pts',(31.3517388718349,5.49099163463111,-2.42092930418135));
#30018=CARTESIAN_POINT('Ctrl Pts',(31.3939161850971,5.44520068393954,-2.51987886844277));
#30019=CARTESIAN_POINT('Ctrl Pts',(31.436608060703,5.39885108460289,-2.62003561532806));
#30020=CARTESIAN_POINT('Ctrl Pts',(31.4807206567692,5.35001548035485,-2.71832462698763));
#30021=CARTESIAN_POINT('Ctrl Pts',(31.5259829068312,5.29872070791517,-2.81488167771062));
#30022=CARTESIAN_POINT('Ctrl Pts',(31.5697886823089,5.24907652801694,-2.90833166039983));
#30023=CARTESIAN_POINT('Ctrl Pts',(31.6146713137554,5.197128415931,-3.00015966435589));
#30024=CARTESIAN_POINT('Ctrl Pts',(31.6603850692973,5.14285714285714,-3.09047252182628));
#30025=CARTESIAN_POINT('',(-60.4312629272455,5.14285714285714,-3.09047252182628));
#30026=CARTESIAN_POINT('Origin',(31.2718056654608,0.,0.));
#30027=CARTESIAN_POINT('',(29.8656463748335,-6.5669102351073,-0.377955629499295));
#30028=CARTESIAN_POINT('',(29.8656463748335,6.5669102351073,-0.377955629499269));
#30029=CARTESIAN_POINT('Origin',(29.8656463748335,0.,0.));
#30030=CARTESIAN_POINT('Ctrl Pts',(29.8656463748335,6.56691023510728,-0.377955629499269));
#30031=CARTESIAN_POINT('Ctrl Pts',(29.8725075439928,6.5601223945667,-0.377832908785134));
#30032=CARTESIAN_POINT('Ctrl Pts',(29.8790313233221,6.55371594181744,-0.378533417250872));
#30033=CARTESIAN_POINT('Ctrl Pts',(29.8852810759567,6.54761680930762,-0.379843594119964));
#30034=CARTESIAN_POINT('Ctrl Pts',(29.8918523561381,6.54120389812085,-0.381221174929515));
#30035=CARTESIAN_POINT('Ctrl Pts',(29.8981209111568,6.53513071591201,-0.3832764131639));
#30036=CARTESIAN_POINT('Ctrl Pts',(29.9041291486039,6.52934354017054,-0.385782549958447));
#30037=CARTESIAN_POINT('Ctrl Pts',(29.9075083267445,6.52608869248297,-0.387192061940608));
#30038=CARTESIAN_POINT('Ctrl Pts',(29.9108045893958,6.52292489077237,-0.388744297301114));
#30039=CARTESIAN_POINT('Ctrl Pts',(29.9140210253342,6.51984677993087,-0.39039428080563));
#30040=CARTESIAN_POINT('Ctrl Pts',(29.9204153242607,6.51372747234116,-0.393674460468415));
#30041=CARTESIAN_POINT('Ctrl Pts',(29.9265008152716,6.50793946229219,-0.397332941703034));
#30042=CARTESIAN_POINT('Ctrl Pts',(29.9324249507833,6.50233824792647,-0.401361685578881));
#30043=CARTESIAN_POINT('Ctrl Pts',(29.9373301272236,6.49770044977186,-0.404697480228541));
#30044=CARTESIAN_POINT('Ctrl Pts',(29.9421235535095,6.49319187366407,-0.40828778998665));
#30045=CARTESIAN_POINT('Ctrl Pts',(29.9469087678782,6.48871046304552,-0.41211279361687));
#30046=CARTESIAN_POINT('Ctrl Pts',(29.9479028070629,6.48777953343309,-0.412907366899729));
#30047=CARTESIAN_POINT('Ctrl Pts',(29.9488966014781,6.48684966489765,-0.413711988676514));
#30048=CARTESIAN_POINT('Ctrl Pts',(29.9498912775077,6.48591974131433,-0.414526339789525));
#30049=CARTESIAN_POINT('Ctrl Pts',(29.9576241534814,6.47869026807829,-0.42085732190663));
#30050=CARTESIAN_POINT('Ctrl Pts',(29.9654019249319,6.47146767959501,-0.427811739749593));
#30051=CARTESIAN_POINT('Ctrl Pts',(29.9733209196286,6.46417108245538,-0.435510985707953));
#30052=CARTESIAN_POINT('Ctrl Pts',(29.9829182505443,6.45532805881548,-0.44484199476825));
#30053=CARTESIAN_POINT('Ctrl Pts',(29.9919885021345,6.44705359857573,-0.454544762727445));
#30054=CARTESIAN_POINT('Ctrl Pts',(30.0008134547635,6.43906208798889,-0.464442747702182));
#30055=CARTESIAN_POINT('Ctrl Pts',(30.0025614062969,6.43747921567539,-0.466403233921351));
#30056=CARTESIAN_POINT('Ctrl Pts',(30.0042998323013,6.43590734417065,-0.468371296570632));
#30057=CARTESIAN_POINT('Ctrl Pts',(30.0060310804752,6.4343440929234,-0.470345432705976));
#30058=CARTESIAN_POINT('Ctrl Pts',(30.0191369783573,6.42250996566295,-0.485290041447687));
#30059=CARTESIAN_POINT('Ctrl Pts',(30.031839751297,6.41116861900765,-0.500703061129736));
#30060=CARTESIAN_POINT('Ctrl Pts',(30.0443550852513,6.40011900637697,-0.516607199583796));
#30061=CARTESIAN_POINT('Ctrl Pts',(30.0506060384155,6.39460012759283,-0.52455073708397));
#30062=CARTESIAN_POINT('Ctrl Pts',(30.0568106516791,6.38915364007045,-0.532616634573869));
#30063=CARTESIAN_POINT('Ctrl Pts',(30.0629994771853,6.38375101060815,-0.540806413681568));
#30064=CARTESIAN_POINT('Ctrl Pts',(30.0748370591151,6.37341721321275,-0.556471289202405));
#30065=CARTESIAN_POINT('Ctrl Pts',(30.0864049630046,6.36342886769562,-0.572310950518507));
#30066=CARTESIAN_POINT('Ctrl Pts',(30.0979191698185,6.35357062888264,-0.588245141470827));
#30067=CARTESIAN_POINT('Ctrl Pts',(30.1211338537217,6.3336946702878,-0.620371297635091));
#30068=CARTESIAN_POINT('Ctrl Pts',(30.1439826702986,6.31449626551089,-0.652929314975647));
#30069=CARTESIAN_POINT('Ctrl Pts',(30.166659015077,6.29578657510829,-0.685777462655701));
#30070=CARTESIAN_POINT('Ctrl Pts',(30.1868553837943,6.27912305152682,-0.715033205091633));
#30071=CARTESIAN_POINT('Ctrl Pts',(30.2069158355587,6.26284623933258,-0.744518847551107));
#30072=CARTESIAN_POINT('Ctrl Pts',(30.2269993156952,6.24679677088334,-0.774128879324885));
#30073=CARTESIAN_POINT('Ctrl Pts',(30.2389447497761,6.23725072278359,-0.791740602008511));
#30074=CARTESIAN_POINT('Ctrl Pts',(30.2508989662365,6.22778417331905,-0.809398803531555));
#30075=CARTESIAN_POINT('Ctrl Pts',(30.2629011553761,6.21835795433208,-0.827084782242122));
#30076=CARTESIAN_POINT('Ctrl Pts',(30.302268731467,6.18743964527177,-0.885095375520649));
#30077=CARTESIAN_POINT('Ctrl Pts',(30.3420024626169,6.15710898525446,-0.943463646964114));
#30078=CARTESIAN_POINT('Ctrl Pts',(30.3821258030208,6.12732774116849,-1.00198727566907));
#30079=CARTESIAN_POINT('Ctrl Pts',(30.4277433739611,6.09346844627666,-1.06852475129435));
#30080=CARTESIAN_POINT('Ctrl Pts',(30.4738648259364,6.06031882234849,-1.1352629705455));
#30081=CARTESIAN_POINT('Ctrl Pts',(30.5205608459579,6.02776378653948,-1.20191078358617));
#30082=CARTESIAN_POINT('Ctrl Pts',(30.5330992620028,6.01902238666983,-1.21980648450457));
#30083=CARTESIAN_POINT('Ctrl Pts',(30.5456792644843,6.01032359736377,-1.23769570207054));
#30084=CARTESIAN_POINT('Ctrl Pts',(30.5583025227219,6.00166470917368,-1.25557287713379));
#30085=CARTESIAN_POINT('Ctrl Pts',(30.5681724071966,5.99489448990794,-1.26955069880942));
#30086=CARTESIAN_POINT('Ctrl Pts',(30.5780684551723,5.98814840962004,-1.28352288344113));
#30087=CARTESIAN_POINT('Ctrl Pts',(30.5879926334101,5.98142414590736,-1.29748907624301));
#30088=CARTESIAN_POINT('Ctrl Pts',(30.6669544011375,5.92792251215015,-1.40861115059904));
#30089=CARTESIAN_POINT('Ctrl Pts',(30.7475298903906,5.87599870594709,-1.51939708458653));
#30090=CARTESIAN_POINT('Ctrl Pts',(30.8293107323995,5.82574321254352,-1.63008315076544));
#30091=CARTESIAN_POINT('Ctrl Pts',(30.9214154700563,5.76914353807153,-1.75474206643868));
#30092=CARTESIAN_POINT('Ctrl Pts',(31.0150485279702,5.71466041937621,-1.87927598022933));
#30093=CARTESIAN_POINT('Ctrl Pts',(31.1095944938123,5.66237027343985,-2.0040523816082));
#30094=CARTESIAN_POINT('Ctrl Pts',(31.1634082906049,5.63260769962077,-2.07507277733319));
#30095=CARTESIAN_POINT('Ctrl Pts',(31.2175173246529,5.60355460236516,-2.14617211425946));
#30096=CARTESIAN_POINT('Ctrl Pts',(31.2718056654608,5.57521816165486,-2.21741796916003));
#30097=CARTESIAN_POINT('Ctrl Pts',(31.2718056654608,-5.57521816165487,-2.21741796916002));
#30098=CARTESIAN_POINT('Ctrl Pts',(31.1819875314053,-5.62209979760386,-2.09954422960071));
#30099=CARTESIAN_POINT('Ctrl Pts',(31.0927465664112,-5.67089537566277,-1.98218339393731));
#30100=CARTESIAN_POINT('Ctrl Pts',(31.0046065204154,-5.72156004652258,-1.86503220805667));
#30101=CARTESIAN_POINT('Ctrl Pts',(30.9255422977669,-5.76700775161531,-1.75994413668838));
#30102=CARTESIAN_POINT('Ctrl Pts',(30.8473642922524,-5.81395915530375,-1.65502294282812));
#30103=CARTESIAN_POINT('Ctrl Pts',(30.7704327542947,-5.86234777851516,-1.55005512612116));
#30104=CARTESIAN_POINT('Ctrl Pts',(30.7086828848192,-5.90118739158838,-1.46580165670074));
#30105=CARTESIAN_POINT('Ctrl Pts',(30.6477358551072,-5.94095238471506,-1.38151794451207));
#30106=CARTESIAN_POINT('Ctrl Pts',(30.5877661622583,-5.98159134441235,-1.29710698186777));
#30107=CARTESIAN_POINT('Ctrl Pts',(30.5783243505759,-5.98798966640143,-1.28381706198719));
#30108=CARTESIAN_POINT('Ctrl Pts',(30.5689093564766,-5.99440681250476,-1.27052356904323));
#30109=CARTESIAN_POINT('Ctrl Pts',(30.5595195554009,-6.00084470060566,-1.25722696506484));
#30110=CARTESIAN_POINT('Ctrl Pts',(30.5031524419472,-6.03949143721509,-1.17740725653641));
#30111=CARTESIAN_POINT('Ctrl Pts',(30.4476477085009,-6.0789178589505,-1.09741768380242));
#30112=CARTESIAN_POINT('Ctrl Pts',(30.3926547385931,-6.1195304846082,-1.01734187625657));
#30113=CARTESIAN_POINT('Ctrl Pts',(30.3490261759155,-6.15175042993903,-0.953813894510328));
#30114=CARTESIAN_POINT('Ctrl Pts',(30.3057199242426,-6.18471646153748,-0.890231728104117));
#30115=CARTESIAN_POINT('Ctrl Pts',(30.2625722572727,-6.21861100640185,-0.826639841079345));
#30116=CARTESIAN_POINT('Ctrl Pts',(30.2509982419382,-6.22770294600282,-0.809581827813351));
#30117=CARTESIAN_POINT('Ctrl Pts',(30.2394493761657,-6.23684780069786,-0.792518945606304));
#30118=CARTESIAN_POINT('Ctrl Pts',(30.227886703887,-6.24608463641092,-0.77546319513685));
#30119=CARTESIAN_POINT('Ctrl Pts',(30.2052208675914,-6.26419122986221,-0.742029501028785));
#30120=CARTESIAN_POINT('Ctrl Pts',(30.182685244376,-6.28250490217154,-0.708903832679339));
#30121=CARTESIAN_POINT('Ctrl Pts',(30.1600108241324,-6.30128103849979,-0.676163278587289));
#30122=CARTESIAN_POINT('Ctrl Pts',(30.1393594431902,-6.31838194515021,-0.646343876479036));
#30123=CARTESIAN_POINT('Ctrl Pts',(30.1185934610269,-6.3358659017507,-0.616843789210932));
#30124=CARTESIAN_POINT('Ctrl Pts',(30.097535297881,-6.35389930559972,-0.587714258355697));
#30125=CARTESIAN_POINT('Ctrl Pts',(30.086119151503,-6.36367565582589,-0.571922425712827));
#30126=CARTESIAN_POINT('Ctrl Pts',(30.0746477525123,-6.37358221414102,-0.556221757231938));
#30127=CARTESIAN_POINT('Ctrl Pts',(30.0629107652948,-6.38382864590174,-0.54069175867353));
#30128=CARTESIAN_POINT('Ctrl Pts',(30.0534369671071,-6.39209930555624,-0.528156338001143));
#30129=CARTESIAN_POINT('Ctrl Pts',(30.043919380635,-6.40047911568583,-0.51590652917707));
#30130=CARTESIAN_POINT('Ctrl Pts',(30.0343494281368,-6.4089793588288,-0.504052250919162));
#30131=CARTESIAN_POINT('Ctrl Pts',(30.0254564440403,-6.4168783036879,-0.493036531871049));
#30132=CARTESIAN_POINT('Ctrl Pts',(30.0165182973371,-6.4248811549012,-0.482362363619343));
#30133=CARTESIAN_POINT('Ctrl Pts',(30.007561954601,-6.43296147857311,-0.472106200546239));
#30134=CARTESIAN_POINT('Ctrl Pts',(30.0068801630943,-6.43357658411489,-0.471325461679847));
#30135=CARTESIAN_POINT('Ctrl Pts',(30.0061982830898,-6.43419212095116,-0.470547139131873));
#30136=CARTESIAN_POINT('Ctrl Pts',(30.0055163349455,-6.4348080686191,-0.469771263647443));
#30137=CARTESIAN_POINT('Ctrl Pts',(29.999426485346,-6.4403085288674,-0.462842635645629));
#30138=CARTESIAN_POINT('Ctrl Pts',(29.9933391033403,-6.44583328872601,-0.456096771562847));
#30139=CARTESIAN_POINT('Ctrl Pts',(29.987190434343,-6.45144755712158,-0.449605478393239));
#30140=CARTESIAN_POINT('Ctrl Pts',(29.9834438098157,-6.45486855045898,-0.44565007955589));
#30141=CARTESIAN_POINT('Ctrl Pts',(29.9796750763159,-6.45832211622899,-0.441788848226876));
#30142=CARTESIAN_POINT('Ctrl Pts',(29.9758760317652,-6.46181664631018,-0.438034612133003));
#30143=CARTESIAN_POINT('Ctrl Pts',(29.9672827168783,-6.46972115939749,-0.42954265251402));
#30144=CARTESIAN_POINT('Ctrl Pts',(29.9585336198971,-6.47783579642184,-0.421599175152793));
#30145=CARTESIAN_POINT('Ctrl Pts',(29.9494315602762,-6.48634799335753,-0.414175830172066));
#30146=CARTESIAN_POINT('Ctrl Pts',(29.9443612126388,-6.49108975504875,-0.410040618884511));
#30147=CARTESIAN_POINT('Ctrl Pts',(29.9391527039694,-6.49597193326323,-0.405860302400109));
#30148=CARTESIAN_POINT('Ctrl Pts',(29.9337071438672,-6.50110604110052,-0.401902571557844));
#30149=CARTESIAN_POINT('Ctrl Pts',(29.927097252935,-6.50733788726545,-0.397098626928533));
#30150=CARTESIAN_POINT('Ctrl Pts',(29.9201388905088,-6.51394006959045,-0.392621605951022));
#30151=CARTESIAN_POINT('Ctrl Pts',(29.9126651940782,-6.5210985400584,-0.38887619517018));
#30152=CARTESIAN_POINT('Ctrl Pts',(29.9048166960573,-6.52861600371532,-0.384942954186471));
#30153=CARTESIAN_POINT('Ctrl Pts',(29.8964014607698,-6.53674516224513,-0.381812401352293));
#30154=CARTESIAN_POINT('Ctrl Pts',(29.8872163718764,-6.54571003340667,-0.379924022087368));
#30155=CARTESIAN_POINT('Ctrl Pts',(29.8804719643197,-6.55229273995512,-0.378537426973039));
#30156=CARTESIAN_POINT('Ctrl Pts',(29.8733123700361,-6.55932610303385,-0.377819678470141));
#30157=CARTESIAN_POINT('Ctrl Pts',(29.8656463748432,-6.56691023509677,-0.377955629499085));
#30158=CARTESIAN_POINT('Origin',(23.3621596556826,0.,0.));
#30159=CARTESIAN_POINT('',(23.3560798022767,9.24999809463599,-6.60452283141046E-10));
#30160=CARTESIAN_POINT('Ctrl Pts',(23.3560798282383,9.24999837277875,-6.67384040739516E-9));
#30161=CARTESIAN_POINT('Ctrl Pts',(23.3566780177678,9.24999837572821,-0.0102225537292777));
#30162=CARTESIAN_POINT('Ctrl Pts',(23.3670051565122,9.24999029805898,-0.0157301067324773));
#30163=CARTESIAN_POINT('Ctrl Pts',(23.375414584291,9.24996826963113,-0.0202809688865867));
#30164=CARTESIAN_POINT('Ctrl Pts',(23.3754183438715,9.24996825978294,-0.0202830034284274));
#30165=CARTESIAN_POINT('Ctrl Pts',(23.3754221035694,9.24996824993205,-0.0202850377621649));
#30166=CARTESIAN_POINT('Ctrl Pts',(23.3754258633847,9.24996824007846,-0.0202870718878598));
#30167=CARTESIAN_POINT('Ctrl Pts',(23.3838350809832,9.24994620151217,-0.0248366054593298));
#30168=CARTESIAN_POINT('Ctrl Pts',(23.3928310844359,9.24991067376018,-0.0283456960327398));
#30169=CARTESIAN_POINT('Ctrl Pts',(23.4018732133928,9.2498611248735,-0.0314960934238296));
#30170=CARTESIAN_POINT('Ctrl Pts',(23.401878048676,9.24986109837721,-0.0314977781005028));
#30171=CARTESIAN_POINT('Ctrl Pts',(23.401882883983,9.24986107187696,-0.0314994626675972));
#30172=CARTESIAN_POINT('Ctrl Pts',(23.4018877193138,9.24986104537276,-0.0315011471251339));
#30173=CARTESIAN_POINT('Ctrl Pts',(23.4199770283062,9.24976189130746,-0.0378028200424206));
#30174=CARTESIAN_POINT('Ctrl Pts',(23.4383987060992,9.24960739037706,-0.0425720268385514));
#30175=CARTESIAN_POINT('Ctrl Pts',(23.4569145494441,9.24939573886127,-0.0469039022173839));
#30176=CARTESIAN_POINT('Ctrl Pts',(23.4569194598224,9.24939568273156,-0.0469050510252594));
#30177=CARTESIAN_POINT('Ctrl Pts',(23.4569243702082,9.24939562659782,-0.0469061997977794));
#30178=CARTESIAN_POINT('Ctrl Pts',(23.4569292806017,9.24939557046007,-0.0469073485349474));
#30179=CARTESIAN_POINT('Ctrl Pts',(23.4939660705805,9.24897214978062,-0.0555717330220713));
#30180=CARTESIAN_POINT('Ctrl Pts',(23.5314364698805,9.2483200844845,-0.0622254714305722));
#30181=CARTESIAN_POINT('Ctrl Pts',(23.569035993724,9.24743432044532,-0.0682690984893951));
#30182=CARTESIAN_POINT('Ctrl Pts',(23.5690408995974,9.24743420487348,-0.0682698870437648));
#30183=CARTESIAN_POINT('Ctrl Pts',(23.5690458054721,9.24743408929769,-0.0682706755863066));
#30184=CARTESIAN_POINT('Ctrl Pts',(23.5690507113481,9.24743397371795,-0.0682714641170214));
#30185=CARTESIAN_POINT('Ctrl Pts',(23.6442548651033,9.24566220524802,-0.0803591696110631));
#30186=CARTESIAN_POINT('Ctrl Pts',(23.719780223829,9.24296231063544,-0.0896678135679566));
#30187=CARTESIAN_POINT('Ctrl Pts',(23.7952824304768,9.23933323520794,-0.098112337331162));
#30188=CARTESIAN_POINT('Ctrl Pts',(23.795287196916,9.23933300610514,-0.0981128704322552));
#30189=CARTESIAN_POINT('Ctrl Pts',(23.7952919633553,9.23933277699862,-0.0981134035295249));
#30190=CARTESIAN_POINT('Ctrl Pts',(23.7952967297948,9.23933254788841,-0.0981139366229708));
#30191=CARTESIAN_POINT('Ctrl Pts',(23.9463062361403,9.23207391784971,-0.115003310510118));
#30192=CARTESIAN_POINT('Ctrl Pts',(24.0974556990499,9.22109573441987,-0.128054897542612));
#30193=CARTESIAN_POINT('Ctrl Pts',(24.2484785175586,9.20637641464955,-0.139900632118544));
#30194=CARTESIAN_POINT('Ctrl Pts',(24.2484829666272,9.2063759810246,-0.139900981088888));
#30195=CARTESIAN_POINT('Ctrl Pts',(24.2484874156951,9.20637554739644,-0.139901330058036));
#30196=CARTESIAN_POINT('Ctrl Pts',(24.2484918647625,9.20637511376508,-0.139901679025988));
#30197=CARTESIAN_POINT('Ctrl Pts',(24.5505425107233,9.17693554307987,-0.163593384587027));
#30198=CARTESIAN_POINT('Ctrl Pts',(24.8500228881277,9.13271031628177,-0.181771961304202));
#30199=CARTESIAN_POINT('Ctrl Pts',(25.1449954475175,9.07440073882145,-0.198110501056529));
#30200=CARTESIAN_POINT('Ctrl Pts',(25.1449991716412,9.07440000264425,-0.19811070733586));
#30201=CARTESIAN_POINT('Ctrl Pts',(25.1450028957642,9.0743992664648,-0.198110913614874));
#30202=CARTESIAN_POINT('Ctrl Pts',(25.1450066198866,9.07439853028311,-0.198111119893571));
#30203=CARTESIAN_POINT('Ctrl Pts',(25.734956508507,8.95777768468516,-0.23078837411552));
#30204=CARTESIAN_POINT('Ctrl Pts',(26.3094088549805,8.78499087735302,-0.255519529851774));
#30205=CARTESIAN_POINT('Ctrl Pts',(26.8679234097883,8.55541116229534,-0.27759745040406));
#30206=CARTESIAN_POINT('Ctrl Pts',(26.867925760244,8.5554101961308,-0.277597543316903));
#30207=CARTESIAN_POINT('Ctrl Pts',(26.8679281106996,8.55540922996518,-0.277597636229693));
#30208=CARTESIAN_POINT('Ctrl Pts',(26.8679304611549,8.5554082637985,-0.277597729142428));
#30209=CARTESIAN_POINT('Ctrl Pts',(27.1471871052162,8.44061839374216,-0.288636653344279));
#30210=CARTESIAN_POINT('Ctrl Pts',(27.4237272806306,8.31073561236966,-0.298912461553731));
#30211=CARTESIAN_POINT('Ctrl Pts',(27.6907408700783,8.16889014503095,-0.308412822043665));
#30212=CARTESIAN_POINT('Ctrl Pts',(27.6907425556339,8.16888924961423,-0.308412882015843));
#30213=CARTESIAN_POINT('Ctrl Pts',(27.6907442411893,8.16888835419702,-0.308412941987992));
#30214=CARTESIAN_POINT('Ctrl Pts',(27.6907459267443,8.16888745877932,-0.308413001960112));
#30215=CARTESIAN_POINT('Ctrl Pts',(27.9577599700424,8.02704153892829,-0.317913373144742));
#30216=CARTESIAN_POINT('Ctrl Pts',(28.2162196174067,7.8729946215703,-0.326677439449265));
#30217=CARTESIAN_POINT('Ctrl Pts',(28.4663064740913,7.7070127601481,-0.334872469822339));
#30218=CARTESIAN_POINT('Ctrl Pts',(28.4663075265582,7.70701206162913,-0.33487250431035));
#30219=CARTESIAN_POINT('Ctrl Pts',(28.4663085790249,7.70701136310996,-0.33487253879835));
#30220=CARTESIAN_POINT('Ctrl Pts',(28.4663096314915,7.70701066459057,-0.33487257328634));
#30221=CARTESIAN_POINT('Ctrl Pts',(28.9070555201026,7.4144887448157,-0.34931525499634));
#30222=CARTESIAN_POINT('Ctrl Pts',(29.3219854583099,7.08516810894049,-0.362013648044849));
#30223=CARTESIAN_POINT('Ctrl Pts',(29.7101085977472,6.71766015929422,-0.373413798110151));
#30224=CARTESIAN_POINT('Ctrl Pts',(29.7624427821908,6.66810570899995,-0.374950984367759));
#30225=CARTESIAN_POINT('Ctrl Pts',(29.8142895317361,6.6178568890955,-0.376464564268085));
#30226=CARTESIAN_POINT('Ctrl Pts',(29.8656463748334,6.56691023510737,-0.377955629499264));
#30227=CARTESIAN_POINT('',(23.3621597248275,-9.24999241530675,-0.0116776286864305));
#30228=CARTESIAN_POINT('Ctrl Pts',(29.8656463748335,-6.5669102351073,-0.377955629499294));
#30229=CARTESIAN_POINT('Ctrl Pts',(29.4847714407085,-6.94474310627589,-0.366897524338192));
#30230=CARTESIAN_POINT('Ctrl Pts',(29.0769538041632,-7.28419815787297,-0.354601205857789));
#30231=CARTESIAN_POINT('Ctrl Pts',(28.6431883543724,-7.58666973512015,-0.340620835122163));
#30232=CARTESIAN_POINT('Ctrl Pts',(28.5846997977317,-7.62745473998063,-0.338735734070377));
#30233=CARTESIAN_POINT('Ctrl Pts',(28.5257394240778,-7.66756726314656,-0.336820011942593));
#30234=CARTESIAN_POINT('Ctrl Pts',(28.4663096314912,-7.70701066459059,-0.334872573291177));
#30235=CARTESIAN_POINT('Ctrl Pts',(28.4663085790239,-7.70701136311043,-0.334872538803164));
#30236=CARTESIAN_POINT('Ctrl Pts',(28.4663075265564,-7.70701206163006,-0.334872504315141));
#30237=CARTESIAN_POINT('Ctrl Pts',(28.4663064740889,-7.70701276014948,-0.334872469827109));
#30238=CARTESIAN_POINT('Ctrl Pts',(28.2162196174051,-7.87299462157124,-0.326677439449156));
#30239=CARTESIAN_POINT('Ctrl Pts',(27.9577599700418,-8.02704153892891,-0.317913373136687));
#30240=CARTESIAN_POINT('Ctrl Pts',(27.6907459267442,-8.1688874587795,-0.308413001956161));
#30241=CARTESIAN_POINT('Ctrl Pts',(27.6907442411881,-8.16888835419778,-0.308412941984002));
#30242=CARTESIAN_POINT('Ctrl Pts',(27.6907425556317,-8.16888924961559,-0.308412882011813));
#30243=CARTESIAN_POINT('Ctrl Pts',(27.6907408700749,-8.16889014503291,-0.308412822039595));
#30244=CARTESIAN_POINT('Ctrl Pts',(27.4237272806281,-8.31073561237086,-0.298912461553772));
#30245=CARTESIAN_POINT('Ctrl Pts',(27.1471871052143,-8.44061839374265,-0.288636653353161));
#30246=CARTESIAN_POINT('Ctrl Pts',(26.8679304611544,-8.55540826379855,-0.277597729148227));
#30247=CARTESIAN_POINT('Ctrl Pts',(26.8679281106974,-8.55540922996587,-0.27759763623543));
#30248=CARTESIAN_POINT('Ctrl Pts',(26.8679257602403,-8.55541019613213,-0.277597543322579));
#30249=CARTESIAN_POINT('Ctrl Pts',(26.867923409783,-8.55541116229733,-0.277597450409673));
#30250=CARTESIAN_POINT('Ctrl Pts',(26.309408854977,-8.78499087735412,-0.255519529851172));
#30251=CARTESIAN_POINT('Ctrl Pts',(25.7349565085049,-8.9577776846856,-0.23078837411658));
#30252=CARTESIAN_POINT('Ctrl Pts',(25.1450066198861,-9.07439853028321,-0.198111119893957));
#30253=CARTESIAN_POINT('Ctrl Pts',(25.1450028957612,-9.07439926646539,-0.198110913615121));
#30254=CARTESIAN_POINT('Ctrl Pts',(25.1449991716356,-9.07440000264534,-0.198110707335968));
#30255=CARTESIAN_POINT('Ctrl Pts',(25.1449954475095,-9.07440073882304,-0.198110501056499));
#30256=CARTESIAN_POINT('Ctrl Pts',(24.8500228881221,-9.13271031628261,-0.181771961303894));
#30257=CARTESIAN_POINT('Ctrl Pts',(24.5505425107174,-9.1769355430799,-0.163593384622763));
#30258=CARTESIAN_POINT('Ctrl Pts',(24.2484918647611,-9.20637511376504,-0.139901679037309));
#30259=CARTESIAN_POINT('Ctrl Pts',(24.2484874156906,-9.20637554739671,-0.139901330069121));
#30260=CARTESIAN_POINT('Ctrl Pts',(24.2484829666197,-9.20637598102516,-0.139900981099737));
#30261=CARTESIAN_POINT('Ctrl Pts',(24.2484785175481,-9.2063764146504,-0.139900632129157));
#30262=CARTESIAN_POINT('Ctrl Pts',(24.0974556990432,-9.22109573442037,-0.128054897541096));
#30263=CARTESIAN_POINT('Ctrl Pts',(23.9463062361367,-9.2320739178499,-0.115003310509656));
#30264=CARTESIAN_POINT('Ctrl Pts',(23.7952967297941,-9.23933254788843,-0.0981139366229608));
#30265=CARTESIAN_POINT('Ctrl Pts',(23.7952919633514,-9.23933277699881,-0.0981134035291551));
#30266=CARTESIAN_POINT('Ctrl Pts',(23.7952871969089,-9.23933300610547,-0.0981128704315258));
#30267=CARTESIAN_POINT('Ctrl Pts',(23.7952824304665,-9.23933323520843,-0.0981123373300727));
#30268=CARTESIAN_POINT('Ctrl Pts',(23.7197802238219,-9.2429623106357,-0.0896678135672034));
#30269=CARTESIAN_POINT('Ctrl Pts',(23.6442548650996,-9.24566220524811,-0.0803591696095396));
#30270=CARTESIAN_POINT('Ctrl Pts',(23.5690507113475,-9.24743397371796,-0.068271464116656));
#30271=CARTESIAN_POINT('Ctrl Pts',(23.5690458054681,-9.24743408929778,-0.0682706755854086));
#30272=CARTESIAN_POINT('Ctrl Pts',(23.5690408995901,-9.24743420487365,-0.068269887042334));
#30273=CARTESIAN_POINT('Ctrl Pts',(23.5690359937135,-9.24743432044557,-0.0682690984874317));
#30274=CARTESIAN_POINT('Ctrl Pts',(23.5314364698732,-9.24832008448463,-0.0622254714293397));
#30275=CARTESIAN_POINT('Ctrl Pts',(23.4939660705731,-9.24897214983,-0.055571723955567));
#30276=CARTESIAN_POINT('Ctrl Pts',(23.4569292913262,-9.2493955706006,-0.0469072991570471));
#30277=CARTESIAN_POINT('Ctrl Pts',(23.4569243811925,-9.24939562673541,-0.0469061504749738));
#30278=CARTESIAN_POINT('Ctrl Pts',(23.4569194710664,-9.2493956828662,-0.0469050017575602));
#30279=CARTESIAN_POINT('Ctrl Pts',(23.4569145609479,-9.24939573899298,-0.0469038530048031));
#30280=CARTESIAN_POINT('Ctrl Pts',(23.4383987227168,-9.24960739055848,-0.0425719574877666));
#30281=CARTESIAN_POINT('Ctrl Pts',(23.4199770709982,-9.24976189104565,-0.0378028340633931));
#30282=CARTESIAN_POINT('Ctrl Pts',(23.4018877334049,-9.24986104529552,-0.0315011520350705));
#30283=CARTESIAN_POINT('Ctrl Pts',(23.4018828933734,-9.2498610718255,-0.0314994659402038));
#30284=CARTESIAN_POINT('Ctrl Pts',(23.4018780533658,-9.24986109835151,-0.0314977797355663));
#30285=CARTESIAN_POINT('Ctrl Pts',(23.4018732133819,-9.24986112487356,-0.031496093421139));
#30286=CARTESIAN_POINT('Ctrl Pts',(23.3928310750493,-9.24991067381161,-0.0283456927611094));
#30287=CARTESIAN_POINT('Ctrl Pts',(23.3838350766164,-9.24994620152362,-0.0248366031008535));
#30288=CARTESIAN_POINT('Ctrl Pts',(23.3754258633825,-9.24996824007847,-0.0202870718871724));
#30289=CARTESIAN_POINT('Ctrl Pts',(23.3754221035648,-9.24996824993206,-0.0202850377600923));
#30290=CARTESIAN_POINT('Ctrl Pts',(23.3754183438643,-9.24996825978296,-0.0202830034249692));
#30291=CARTESIAN_POINT('Ctrl Pts',(23.3754145842812,-9.24996826963115,-0.0202809688817427));
#30292=CARTESIAN_POINT('Ctrl Pts',(23.3709568489949,-9.24997994663257,-0.0178686122552752));
#30293=CARTESIAN_POINT('Ctrl Pts',(23.3659604527863,-9.249987704137,-0.0151874246645509));
#30294=CARTESIAN_POINT('Ctrl Pts',(23.3621597248275,-9.24999241530675,-0.0116776286864305));
#30295=CARTESIAN_POINT('',(23.3621596556826,-5.66399144605651E-16,9.25));
#30296=CARTESIAN_POINT('Origin',(23.3621596556826,0.,0.));
#30297=CARTESIAN_POINT('',(23.3560798393748,-9.24999818736112,-1.077153489017E-8));
#30298=CARTESIAN_POINT('Ctrl Pts',(23.3621597248275,-9.24999241530675,-0.0116776286864305));
#30299=CARTESIAN_POINT('Ctrl Pts',(23.3587904572015,-9.24999659166241,-0.00856626631297116));
#30300=CARTESIAN_POINT('Ctrl Pts',(23.3563609263675,-9.24999837416356,-0.00480370845307387));
#30301=CARTESIAN_POINT('Ctrl Pts',(23.3560798285161,-9.24999837277875,-1.1406897794386E-8));
#30302=CARTESIAN_POINT('',(16.3220957355182,-6.,0.));
#30303=CARTESIAN_POINT('Origin',(23.3621596556826,0.,0.));
#30304=CARTESIAN_POINT('',(16.3220957355182,6.,0.));
#30305=CARTESIAN_POINT('Origin',(16.3220957355182,0.,0.));
#30306=CARTESIAN_POINT('Origin',(23.3621596556826,0.,0.));
#30307=CARTESIAN_POINT('Origin',(23.3621596556826,0.,0.));
#30308=CARTESIAN_POINT('',(12.9815732451447,2.54439044914164E-11,-11.0119484097524));
#30309=CARTESIAN_POINT('',(23.3608103941008,-11.1532440216953,-5.06593335958171));
#30310=CARTESIAN_POINT('Ctrl Pts',(12.9815732451008,2.5445788709682E-11,
-11.0119484101204));
#30311=CARTESIAN_POINT('Ctrl Pts',(12.9815732274295,-0.383296294064764,
-11.0119485582815));
#30312=CARTESIAN_POINT('Ctrl Pts',(12.9993217484721,-0.765312998797785,
-10.9941006207665));
#30313=CARTESIAN_POINT('Ctrl Pts',(13.0347559988626,-1.1460555907501,-10.9585267749209));
#30314=CARTESIAN_POINT('Ctrl Pts',(13.0368286609663,-1.16832643697724,-10.9564459474346));
#30315=CARTESIAN_POINT('Ctrl Pts',(13.0389618718051,-1.19059290057529,-10.9543044712817));
#30316=CARTESIAN_POINT('Ctrl Pts',(13.0411556343664,-1.21285503798338,-10.9521023639809));
#30317=CARTESIAN_POINT('Ctrl Pts',(13.0673836657568,-1.47901512706784,-10.9257745651442));
#30318=CARTESIAN_POINT('Ctrl Pts',(13.1025879418344,-1.74579707980255,-10.8904589178109));
#30319=CARTESIAN_POINT('Ctrl Pts',(13.1460558221011,-2.00934344707994,-10.8469554421057));
#30320=CARTESIAN_POINT('Ctrl Pts',(13.1611087883244,-2.10060979226513,-10.83189014915));
#30321=CARTESIAN_POINT('Ctrl Pts',(13.1771529803443,-2.19148779862728,-10.81584273198));
#30322=CARTESIAN_POINT('Ctrl Pts',(13.1941594450425,-2.28181600059225,-10.798845827919));
#30323=CARTESIAN_POINT('Ctrl Pts',(13.2023910039891,-2.32553713442028,-10.7906188965626));
#30324=CARTESIAN_POINT('Ctrl Pts',(13.2108484018431,-2.36913426878318,-10.7821685435845));
#30325=CARTESIAN_POINT('Ctrl Pts',(13.2195283907449,-2.4125885817506,-10.7734983679309));
#30326=CARTESIAN_POINT('Ctrl Pts',(13.3201001314545,-2.91607723201734,-10.6730403296062));
#30327=CARTESIAN_POINT('Ctrl Pts',(13.4501508634135,-3.4036814155668,-10.5433923350781));
#30328=CARTESIAN_POINT('Ctrl Pts',(13.6081630039645,-3.87613361463931,-10.3871346982887));
#30329=CARTESIAN_POINT('Ctrl Pts',(13.6691942514409,-4.05861546053914,-10.3267811174328));
#30330=CARTESIAN_POINT('Ctrl Pts',(13.7343973267524,-4.23883645844413,-10.2624577747158));
#30331=CARTESIAN_POINT('Ctrl Pts',(13.8036860977875,-4.41683730799235,-10.1943136878064));
#30332=CARTESIAN_POINT('Ctrl Pts',(13.8328199711978,-4.49168138647981,-10.1656611201245));
#30333=CARTESIAN_POINT('Ctrl Pts',(13.8626775326182,-4.56611464018205,-10.1363412173927));
#30334=CARTESIAN_POINT('Ctrl Pts',(13.8932514259218,-4.64014509869768,-10.1063639362644));
#30335=CARTESIAN_POINT('Ctrl Pts',(13.9943512020743,-4.88494423860655,-10.0072369987289));
#30336=CARTESIAN_POINT('Ctrl Pts',(14.1019598843113,-5.1222638353909,-9.90221549601681));
#30337=CARTESIAN_POINT('Ctrl Pts',(14.2158396515836,-5.35278002273372,-9.79173341205274));
#30338=CARTESIAN_POINT('Ctrl Pts',(14.2236525199707,-5.36859488323034,-9.78415364611349));
#30339=CARTESIAN_POINT('Ctrl Pts',(14.2314949176702,-5.38437771263948,-9.77654816486061));
#30340=CARTESIAN_POINT('Ctrl Pts',(14.2393667732968,-5.40012872553306,-9.76891710267621));
#30341=CARTESIAN_POINT('Ctrl Pts',(14.3650579854142,-5.65162773625904,-9.64707067901238));
#30342=CARTESIAN_POINT('Ctrl Pts',(14.4981847686049,-5.89496716334364,-9.51871404350092));
#30343=CARTESIAN_POINT('Ctrl Pts',(14.6384789849032,-6.13072391768223,-9.38459915056585));
#30344=CARTESIAN_POINT('Ctrl Pts',(14.6737714708389,-6.19003100928071,-9.35086113842561));
#30345=CARTESIAN_POINT('Ctrl Pts',(14.7095174354231,-6.24885832423709,-9.31675895403165));
#30346=CARTESIAN_POINT('Ctrl Pts',(14.7457124150901,-6.30721521168454,-9.28230502718912));
#30347=CARTESIAN_POINT('Ctrl Pts',(14.7998381789771,-6.39448176467667,-9.23078282365662));
#30348=CARTESIAN_POINT('Ctrl Pts',(14.8549715128261,-6.48069604666143,-9.17847475902765));
#30349=CARTESIAN_POINT('Ctrl Pts',(14.9110921849357,-6.56589391149648,-9.12541926115511));
#30350=CARTESIAN_POINT('Ctrl Pts',(15.041685362699,-6.76414991038648,-9.00195876425546));
#30351=CARTESIAN_POINT('Ctrl Pts',(15.1776986530004,-6.95682139014027,-8.87440061067004));
#30352=CARTESIAN_POINT('Ctrl Pts',(15.3191490883084,-7.1441213175117,-8.74313806886841));
#30353=CARTESIAN_POINT('Ctrl Pts',(15.386104712241,-7.2327798180839,-8.68100488867582));
#30354=CARTESIAN_POINT('Ctrl Pts',(15.4543283803757,-7.32029479475722,-8.61799959364879));
#30355=CARTESIAN_POINT('Ctrl Pts',(15.5237866306372,-7.40663268301795,-8.55420191705971));
#30356=CARTESIAN_POINT('Ctrl Pts',(15.631823395544,-7.54092437769016,-8.45496972273705));
#30357=CARTESIAN_POINT('Ctrl Pts',(15.7425934164994,-7.67199804493825,-8.35406036021674));
#30358=CARTESIAN_POINT('Ctrl Pts',(15.8555749280103,-7.79941820934665,-8.25217221569744));
#30359=CARTESIAN_POINT('Ctrl Pts',(15.8893542526762,-7.83751441681426,-8.22170959692655));
#30360=CARTESIAN_POINT('Ctrl Pts',(15.9233310534103,-7.87528429890062,-8.19115961757327));
#30361=CARTESIAN_POINT('Ctrl Pts',(15.9574908972915,-7.91271690993404,-8.16054121449193));
#30362=CARTESIAN_POINT('Ctrl Pts',(16.0364328953598,-7.99922213865137,-8.08978334085214));
#30363=CARTESIAN_POINT('Ctrl Pts',(16.1164661586433,-8.0840494038951,-8.01855942060974));
#30364=CARTESIAN_POINT('Ctrl Pts',(16.1974689739095,-8.167105566649,-7.94705648567565));
#30365=CARTESIAN_POINT('Ctrl Pts',(16.3862511497973,-8.36067319851518,-7.78041438077027));
#30366=CARTESIAN_POINT('Ctrl Pts',(16.5808510409098,-8.54531969831238,-7.6117230894063));
#30367=CARTESIAN_POINT('Ctrl Pts',(16.7815955192347,-8.72152156029507,-7.44211131482556));
#30368=CARTESIAN_POINT('Ctrl Pts',(16.8274598051923,-8.76177857085733,-7.40335994793335));
#30369=CARTESIAN_POINT('Ctrl Pts',(16.8736448373626,-8.80159493353399,-7.36456068417118));
#30370=CARTESIAN_POINT('Ctrl Pts',(16.9201545218898,-8.84097660013473,-7.32572724718514));
#30371=CARTESIAN_POINT('Ctrl Pts',(17.073716166418,-8.97100357298887,-7.19751037134778));
#30372=CARTESIAN_POINT('Ctrl Pts',(17.2308071180094,-9.09628923719283,-7.06890359935271));
#30373=CARTESIAN_POINT('Ctrl Pts',(17.3917693612564,-9.21694196463097,-6.94059501703444));
#30374=CARTESIAN_POINT('Ctrl Pts',(17.4912340889155,-9.29149790044471,-6.8613082356181));
#30375=CARTESIAN_POINT('Ctrl Pts',(17.5922012020707,-9.3642909638437,-6.78213270267914));
#30376=CARTESIAN_POINT('Ctrl Pts',(17.6947656292074,-9.43536158302822,-6.70321570188847));
#30377=CARTESIAN_POINT('Ctrl Pts',(17.8575457281888,-9.54815782972409,-6.5779664555498));
#30378=CARTESIAN_POINT('Ctrl Pts',(18.0243246162118,-9.65661829996039,-6.45333491604299));
#30379=CARTESIAN_POINT('Ctrl Pts',(18.1958339964268,-9.76078864798243,-6.33031238527626));
#30380=CARTESIAN_POINT('Ctrl Pts',(18.3051389765451,-9.82717765717364,-6.25190865445575));
#30381=CARTESIAN_POINT('Ctrl Pts',(18.416470201457,-9.89187030973724,-6.17410893862717));
#30382=CARTESIAN_POINT('Ctrl Pts',(18.5299490632647,-9.95482201107074,-6.09724150236054));
#30383=CARTESIAN_POINT('Ctrl Pts',(18.6919068330151,-10.0446670887139,-5.98753579729915));
#30384=CARTESIAN_POINT('Ctrl Pts',(18.8582821726837,-10.1309242043064,-5.87972874713949));
#30385=CARTESIAN_POINT('Ctrl Pts',(19.028597750893,-10.2129461794984,-5.77597483478962));
#30386=CARTESIAN_POINT('Ctrl Pts',(19.0441752064857,-10.220448098522,-5.76648526267183));
#30387=CARTESIAN_POINT('Ctrl Pts',(19.0597855949024,-10.2279146095031,-5.75702960254959));
#30388=CARTESIAN_POINT('Ctrl Pts',(19.0754285341388,-10.2353452303139,-5.74760950379945));
#30389=CARTESIAN_POINT('Ctrl Pts',(19.1939081940033,-10.2916247704269,-5.6762616529295));
#30390=CARTESIAN_POINT('Ctrl Pts',(19.3144152371265,-10.3459177594171,-5.6068633280272));
#30391=CARTESIAN_POINT('Ctrl Pts',(19.4368829990435,-10.3980330380265,-5.54011236932002));
#30392=CARTESIAN_POINT('Ctrl Pts',(19.5831223220011,-10.4602641341148,-5.46040473969324));
#30393=CARTESIAN_POINT('Ctrl Pts',(19.7324596468288,-10.5195440088144,-5.38432247817642));
#30394=CARTESIAN_POINT('Ctrl Pts',(19.8855045724414,-10.5757459074742,-5.31311389279469));
#30395=CARTESIAN_POINT('Ctrl Pts',(19.8962358389881,-10.5796866951386,-5.30812086014703));
#30396=CARTESIAN_POINT('Ctrl Pts',(19.9069853432655,-10.5836123466384,-5.30315180853967));
#30397=CARTESIAN_POINT('Ctrl Pts',(19.9177532995298,-10.5875228169023,-5.29820717709418));
#30398=CARTESIAN_POINT('Ctrl Pts',(19.9575183005516,-10.6019637981082,-5.27994714058804));
#30399=CARTESIAN_POINT('Ctrl Pts',(19.9975491622602,-10.6162022971217,-5.26201449196818));
#30400=CARTESIAN_POINT('Ctrl Pts',(20.0378492890609,-10.6302309693699,-5.24444185690922));
#30401=CARTESIAN_POINT('Ctrl Pts',(20.1630026639133,-10.6737974743894,-5.18986945832715));
#30402=CARTESIAN_POINT('Ctrl Pts',(20.2908483914919,-10.7153750760828,-5.13872259572955));
#30403=CARTESIAN_POINT('Ctrl Pts',(20.4214038079289,-10.754702500542,-5.0920472070559));
#30404=CARTESIAN_POINT('Ctrl Pts',(20.5928781972893,-10.8063560150289,-5.03074271284645));
#30405=CARTESIAN_POINT('Ctrl Pts',(20.7671691077214,-10.8535702841615,-4.9778372816226));
#30406=CARTESIAN_POINT('Ctrl Pts',(20.94442935131,-10.8960769893133,-4.93523064039145));
#30407=CARTESIAN_POINT('Ctrl Pts',(20.995814496353,-10.9083990597636,-4.9228795999374));
#30408=CARTESIAN_POINT('Ctrl Pts',(21.0474492395618,-10.9203258484385,-4.91139488931843));
#30409=CARTESIAN_POINT('Ctrl Pts',(21.09933747016,-10.9318487261951,-4.90082131360441));
#30410=CARTESIAN_POINT('Ctrl Pts',(21.2255805168313,-10.9598836616254,-4.87509601141239));
#30411=CARTESIAN_POINT('Ctrl Pts',(21.353441387833,-10.9855508187274,-4.85474602453125));
#30412=CARTESIAN_POINT('Ctrl Pts',(21.4828826861467,-11.0087074356192,-4.84043539750503));
#30413=CARTESIAN_POINT('Ctrl Pts',(21.5416752221987,-11.0192252243867,-4.83393547772421));
#30414=CARTESIAN_POINT('Ctrl Pts',(21.6009563602522,-11.0292416622094,-4.8286938697609));
#30415=CARTESIAN_POINT('Ctrl Pts',(21.6605166873071,-11.0387197298414,-4.82474839119763));
#30416=CARTESIAN_POINT('Ctrl Pts',(21.7393049199761,-11.0512576092448,-4.81952919079354));
#30417=CARTESIAN_POINT('Ctrl Pts',(21.8188480608857,-11.0628933590837,-4.81656587560977));
#30418=CARTESIAN_POINT('Ctrl Pts',(21.8984893540544,-11.0735048808963,-4.81597836766281));
#30419=CARTESIAN_POINT('Ctrl Pts',(21.9447446265687,-11.0796680007266,-4.81563714592834));
#30420=CARTESIAN_POINT('Ctrl Pts',(21.9910325842705,-11.0854859487789,-4.81609650321322));
#30421=CARTESIAN_POINT('Ctrl Pts',(22.0372232100108,-11.0909378851566,-4.81737257485754));
#30422=CARTESIAN_POINT('Ctrl Pts',(22.1039899135981,-11.0988184413143,-4.81921708542365));
#30423=CARTESIAN_POINT('Ctrl Pts',(22.1705282673233,-11.1059466127202,-4.82273204984088));
#30424=CARTESIAN_POINT('Ctrl Pts',(22.2367244241683,-11.1123321983582,-4.82784959532291));
#30425=CARTESIAN_POINT('Ctrl Pts',(22.3548448203634,-11.1237266348551,-4.8369813414649));
#30426=CARTESIAN_POINT('Ctrl Pts',(22.47218105154,-11.1327897089269,-4.85123108401182));
#30427=CARTESIAN_POINT('Ctrl Pts',(22.5888357694595,-11.139637195494,-4.87030011174849));
#30428=CARTESIAN_POINT('Ctrl Pts',(22.7297473141248,-11.1479085275624,-4.89333429503368));
#30429=CARTESIAN_POINT('Ctrl Pts',(22.8696658790769,-11.1529476864071,-4.9233902362237));
#30430=CARTESIAN_POINT('Ctrl Pts',(23.0087902947259,-11.1548965106162,-4.95984270507666));
#30431=CARTESIAN_POINT('Ctrl Pts',(23.0499434250456,-11.1554729746126,-4.9706253789458));
#30432=CARTESIAN_POINT('Ctrl Pts',(23.0910270302596,-11.1557788974522,-4.98196805853579));
#30433=CARTESIAN_POINT('Ctrl Pts',(23.1320461648849,-11.1558175993799,-4.99385533031318));
#30434=CARTESIAN_POINT('Ctrl Pts',(23.2085117001587,-11.15588974531,-5.01601490553846));
#30435=CARTESIAN_POINT('Ctrl Pts',(23.2848869024912,-11.1550160733614,-5.04013662844268));
#30436=CARTESIAN_POINT('Ctrl Pts',(23.3608104906557,-11.1532443098673,-5.06593275297875));
#30437=CARTESIAN_POINT('',(23.3622216893479,-11.1611076779314,-5.04898962599655));
#30438=CARTESIAN_POINT('Ctrl Pts',(23.3609338235094,-11.1532508593964,-5.06595631491688));
#30439=CARTESIAN_POINT('Ctrl Pts',(23.3613828231202,-11.1545850969447,-5.06314833543963));
#30440=CARTESIAN_POINT('Ctrl Pts',(23.3617214043993,-11.1559114660996,-5.06032297389091));
#30441=CARTESIAN_POINT('Ctrl Pts',(23.3621711199265,-11.1585366545092,-5.05466150053041));
#30442=CARTESIAN_POINT('Ctrl Pts',(23.3622835506299,-11.1598325219751,-5.05183232221884));
#30443=CARTESIAN_POINT('Ctrl Pts',(23.3622837237339,-11.161116664397,-5.04899369509034));
#30444=CARTESIAN_POINT('',(23.3621596556826,-1.50019232895551E-15,12.25));
#30445=CARTESIAN_POINT('Origin',(23.3621596556826,0.,0.));
#30446=CARTESIAN_POINT('',(23.3621596556826,-1.50019232895551E-15,12.25));
#30447=CARTESIAN_POINT('',(23.3621596556826,11.1611032572144,-5.04898743133702));
#30448=CARTESIAN_POINT('Origin',(23.3621596556826,0.,0.));
#30449=CARTESIAN_POINT('',(23.3608199268969,11.1532686296421,-5.06590764537049));
#30450=CARTESIAN_POINT('Origin',(23.2960504456339,11.1496971587182,-5.05333275681839));
#30451=CARTESIAN_POINT('Ctrl Pts',(23.3608199267208,11.1532599621143,-5.06590352720005));
#30452=CARTESIAN_POINT('Ctrl Pts',(23.2851099168874,11.1550241480784,-5.04018501841967));
#30453=CARTESIAN_POINT('Ctrl Pts',(23.2088153626835,11.1558905993071,-5.01610178142038));
#30454=CARTESIAN_POINT('Ctrl Pts',(23.1319091372516,11.1558170356561,-4.99381659031829));
#30455=CARTESIAN_POINT('Ctrl Pts',(23.0065821941946,11.1556971557966,-4.95750048117918));
#30456=CARTESIAN_POINT('Ctrl Pts',(22.8810022185292,11.1530840174098,-4.92636875508836));
#30457=CARTESIAN_POINT('Ctrl Pts',(22.7549925111962,11.1479188168036,-4.90077017644917));
#30458=CARTESIAN_POINT('Ctrl Pts',(22.6986428750304,11.1456090171775,-4.88932287906862));
#30459=CARTESIAN_POINT('Ctrl Pts',(22.6422072591868,11.142788578058,-4.87898266372752));
#30460=CARTESIAN_POINT('Ctrl Pts',(22.5856696257093,11.1394507867115,-4.86978382109285));
#30461=CARTESIAN_POINT('Ctrl Pts',(22.4680192465019,11.1325051048096,-4.85064175133027));
#30462=CARTESIAN_POINT('Ctrl Pts',(22.3499266942736,11.1233201691922,-4.83644525304962));
#30463=CARTESIAN_POINT('Ctrl Pts',(22.2312576655186,11.1118030090012,-4.82743144527622));
#30464=CARTESIAN_POINT('Ctrl Pts',(22.1656422229571,11.1054348473088,-4.8224474575212));
#30465=CARTESIAN_POINT('Ctrl Pts',(22.0998654322016,11.0983545374085,-4.81905040982186));
#30466=CARTESIAN_POINT('Ctrl Pts',(22.0339388739251,11.0905496356051,-4.81728321117063));
#30467=CARTESIAN_POINT('Ctrl Pts',(21.9082231125919,11.0756664201302,-4.81391332914321));
#30468=CARTESIAN_POINT('Ctrl Pts',(21.7814080631358,11.0580224086786,-4.81659458033227));
#30469=CARTESIAN_POINT('Ctrl Pts',(21.655559184383,11.0379275898652,-4.82508454412653));
#30470=CARTESIAN_POINT('Ctrl Pts',(21.5963315189804,11.0284704598788,-4.82908013582245));
#30471=CARTESIAN_POINT('Ctrl Pts',(21.5373996159708,11.0184845836996,-4.83435441281115));
#30472=CARTESIAN_POINT('Ctrl Pts',(21.4789497009406,11.0080025426114,-4.84087311309483));
#30473=CARTESIAN_POINT('Ctrl Pts',(21.3622279367936,10.9870703936589,-4.85389065463726));
#30474=CARTESIAN_POINT('Ctrl Pts',(21.2470582382663,10.9641488738826,-4.87177728137055));
#30475=CARTESIAN_POINT('Ctrl Pts',(21.1332169561902,10.939307337495,-4.89405377843275));
#30476=CARTESIAN_POINT('Ctrl Pts',(21.1194119170954,10.9362949119956,-4.89675515272537));
#30477=CARTESIAN_POINT('Ctrl Pts',(21.1056264289217,10.9332542308073,-4.89952113826779));
#30478=CARTESIAN_POINT('Ctrl Pts',(21.0918601058164,10.9301854003157,-4.90235092599176));
#30479=CARTESIAN_POINT('Ctrl Pts',(21.0405875008949,10.9187555557478,-4.91289045690887));
#30480=CARTESIAN_POINT('Ctrl Pts',(20.9895925706238,10.9069380473771,-4.92431218409081));
#30481=CARTESIAN_POINT('Ctrl Pts',(20.9388639538911,10.8947409567297,-4.93657125545549));
#30482=CARTESIAN_POINT('Ctrl Pts',(20.8074102624665,10.8631344850081,-4.96833833857571));
#30483=CARTESIAN_POINT('Ctrl Pts',(20.6777434435588,10.8289788908431,-5.00571952389078));
#30484=CARTESIAN_POINT('Ctrl Pts',(20.5496792463686,10.7923623174254,-5.04795262161033));
#30485=CARTESIAN_POINT('Ctrl Pts',(20.5047265821631,10.779509290855,-5.06277714166981));
#30486=CARTESIAN_POINT('Ctrl Pts',(20.4599587538759,10.766349077854,-5.07820447630388));
#30487=CARTESIAN_POINT('Ctrl Pts',(20.4153833864829,10.7528895773077,-5.09419756001321));
#30488=CARTESIAN_POINT('Ctrl Pts',(20.2991843165291,10.7178033506092,-5.13588833142814));
#30489=CARTESIAN_POINT('Ctrl Pts',(20.1850131651627,10.6808901991499,-5.18117061724925));
#30490=CARTESIAN_POINT('Ctrl Pts',(20.0732309971985,10.6424705764709,-5.22913387074176));
#30491=CARTESIAN_POINT('Ctrl Pts',(20.0585888700092,10.637438065364,-5.23541648335201));
#30492=CARTESIAN_POINT('Ctrl Pts',(20.0439876792257,10.6323797376686,-5.24174505771744));
#30493=CARTESIAN_POINT('Ctrl Pts',(20.0294281869367,10.6272963400987,-5.24811751925262));
#30494=CARTESIAN_POINT('Ctrl Pts',(19.9899973548944,10.6135291982364,-5.26537577630607));
#30495=CARTESIAN_POINT('Ctrl Pts',(19.9508410932218,10.5995670286226,-5.28297007979696));
#30496=CARTESIAN_POINT('Ctrl Pts',(19.9119646421441,10.5854198612558,-5.30086579628549));
#30497=CARTESIAN_POINT('Ctrl Pts',(19.7480083757434,10.5257560628042,-5.37633860253939));
#30498=CARTESIAN_POINT('Ctrl Pts',(19.5885629966609,10.4626584233998,-5.45734371365233));
#30499=CARTESIAN_POINT('Ctrl Pts',(19.4328211684122,10.3962938213192,-5.5423457101382));
#30500=CARTESIAN_POINT('Ctrl Pts',(19.3101579098382,10.3440246368829,-5.60929382543577));
#30501=CARTESIAN_POINT('Ctrl Pts',(19.1897728266506,10.2897369292767,-5.67868690341334));
#30502=CARTESIAN_POINT('Ctrl Pts',(19.0714153292625,10.2334524706779,-5.75003405792709));
#30503=CARTESIAN_POINT('Ctrl Pts',(18.9016894757456,10.1527399853161,-5.85234660223623));
#30504=CARTESIAN_POINT('Ctrl Pts',(18.7360444326255,10.0678922918024,-5.95870710056834));
#30505=CARTESIAN_POINT('Ctrl Pts',(18.5737726476335,9.9789494966074,-6.06773813254394));
#30506=CARTESIAN_POINT('Ctrl Pts',(18.5595594347906,9.9711590918922,-6.07728804452661));
#30507=CARTESIAN_POINT('Ctrl Pts',(18.5453721176096,9.96333726613753,-6.08685847237853));
#30508=CARTESIAN_POINT('Ctrl Pts',(18.5312102300213,9.95548404389193,-6.09644850639014));
#30509=CARTESIAN_POINT('Ctrl Pts',(18.3626959381603,9.86203744806967,-6.21056166964706));
#30510=CARTESIAN_POINT('Ctrl Pts',(18.1977580193019,9.76404251905382,-6.32756306619599));
#30511=CARTESIAN_POINT('Ctrl Pts',(18.0368078275233,9.66208005126259,-6.44582473286028));
#30512=CARTESIAN_POINT('Ctrl Pts',(17.9197006049216,9.58789224644732,-6.53187182090825));
#30513=CARTESIAN_POINT('Ctrl Pts',(17.8047043242091,9.51160350435421,-6.61858721812569));
#30514=CARTESIAN_POINT('Ctrl Pts',(17.6919753333826,9.43343009819351,-6.70535921700973));
#30515=CARTESIAN_POINT('Ctrl Pts',(17.5883305698321,9.36155626930474,-6.78513872396007));
#30516=CARTESIAN_POINT('Ctrl Pts',(17.4864140067132,9.2879885748002,-6.86510597982913));
#30517=CARTESIAN_POINT('Ctrl Pts',(17.3861179794197,9.21269994086293,-6.94510382222357));
#30518=CARTESIAN_POINT('Ctrl Pts',(17.2254565845855,9.09209718849146,-7.07325012362394));
#30519=CARTESIAN_POINT('Ctrl Pts',(17.0689261099161,8.9670795142694,-7.20146744901835));
#30520=CARTESIAN_POINT('Ctrl Pts',(16.9161092582584,8.83754773326068,-7.32910760378148));
#30521=CARTESIAN_POINT('Ctrl Pts',(16.6930329813764,8.64846212436436,-7.51543188802323));
#30522=CARTESIAN_POINT('Ctrl Pts',(16.4778927674604,8.44975933189865,-7.70056120823172));
#30523=CARTESIAN_POINT('Ctrl Pts',(16.2700797258884,8.24082475266365,-7.88311972782491));
#30524=CARTESIAN_POINT('Ctrl Pts',(16.2451498490466,8.21576033279412,-7.90501999633286));
#30525=CARTESIAN_POINT('Ctrl Pts',(16.2203254556708,8.19054866644283,-7.92688331677123));
#30526=CARTESIAN_POINT('Ctrl Pts',(16.1956055245316,8.16518869245223,-7.94870735251825));
#30527=CARTESIAN_POINT('Ctrl Pts',(16.1143868569095,8.08186712950576,-8.02041139956956));
#30528=CARTESIAN_POINT('Ctrl Pts',(16.0342970299172,7.99694590666152,-8.09169455136918));
#30529=CARTESIAN_POINT('Ctrl Pts',(15.9553273945879,7.91036482251391,-8.16248802407884));
#30530=CARTESIAN_POINT('Ctrl Pts',(15.8085457471954,7.74943569942454,-8.29407255661014));
#30531=CARTESIAN_POINT('Ctrl Pts',(15.6656492987518,7.58280910265095,-8.42393082265112));
#30532=CARTESIAN_POINT('Ctrl Pts',(15.526601377284,7.41012613622904,-8.55162007876201));
#30533=CARTESIAN_POINT('Ctrl Pts',(15.456949520793,7.32362581987266,-8.61558215491674));
#30534=CARTESIAN_POINT('Ctrl Pts',(15.3881779253208,7.23545626402979,-8.67908460554051));
#30535=CARTESIAN_POINT('Ctrl Pts',(15.3204539043479,7.14580024918789,-8.74192602992363));
#30536=CARTESIAN_POINT('Ctrl Pts',(15.2020808298621,6.98909280668051,-8.85176493940411));
#30537=CARTESIAN_POINT('Ctrl Pts',(15.0867965419355,6.82769861550008,-8.95968226768334));
#30538=CARTESIAN_POINT('Ctrl Pts',(14.9755957300485,6.66270594177808,-9.06451837904925));
#30539=CARTESIAN_POINT('Ctrl Pts',(14.9539590767423,6.63060285530961,-9.08491663475525));
#30540=CARTESIAN_POINT('Ctrl Pts',(14.9324769028097,6.59836358094115,-9.10519833700311));
#30541=CARTESIAN_POINT('Ctrl Pts',(14.9111563563958,6.56599618907879,-9.12535509869311));
#30542=CARTESIAN_POINT('Ctrl Pts',(14.8542099711004,6.47954409107802,-9.17919305834126));
#30543=CARTESIAN_POINT('Ctrl Pts',(14.7983371386927,6.39212622784975,-9.23220633207766));
#30544=CARTESIAN_POINT('Ctrl Pts',(14.7435645673992,6.30373776682969,-9.28434781086118));
#30545=CARTESIAN_POINT('Ctrl Pts',(14.6043711417208,6.07911634794631,-9.4168548464161));
#30546=CARTESIAN_POINT('Ctrl Pts',(14.4720730873876,5.84799897797753,-9.54385347643406));
#30547=CARTESIAN_POINT('Ctrl Pts',(14.3469550072385,5.61004377135711,-9.66472083458997));
#30548=CARTESIAN_POINT('Ctrl Pts',(14.2258003780593,5.3796264345101,-9.78175939480288));
#30549=CARTESIAN_POINT('Ctrl Pts',(14.1113780347061,5.14279752758011,-9.89304884696983));
#30550=CARTESIAN_POINT('Ctrl Pts',(14.0039217361569,4.8992787262995,-9.99805135858468));
#30551=CARTESIAN_POINT('Ctrl Pts',(13.966473477019,4.81441301532281,-10.0346444789338));
#30552=CARTESIAN_POINT('Ctrl Pts',(13.9298710234828,4.72873511154457,-10.0704743084635));
#30553=CARTESIAN_POINT('Ctrl Pts',(13.8941235352153,4.64223422283333,-10.105518955736));
#30554=CARTESIAN_POINT('Ctrl Pts',(13.8633808025043,4.56784371793926,-10.135657247299));
#30555=CARTESIAN_POINT('Ctrl Pts',(13.8332549565531,4.49273580938441,-10.1652337840266));
#30556=CARTESIAN_POINT('Ctrl Pts',(13.8037941933816,4.41701904105506,-10.1941954693875));
#30557=CARTESIAN_POINT('Ctrl Pts',(13.7296166127968,4.22637609498908,-10.2671164503283));
#30558=CARTESIAN_POINT('Ctrl Pts',(13.6595331492794,4.03154156271738,-10.3362641811527));
#30559=CARTESIAN_POINT('Ctrl Pts',(13.594367561952,3.83431176397562,-10.4007299350271));
#30560=CARTESIAN_POINT('Ctrl Pts',(13.5639648018699,3.74229494193609,-10.4308061904395));
#30561=CARTESIAN_POINT('Ctrl Pts',(13.5346320185754,3.64975685375333,-10.4598638090668));
#30562=CARTESIAN_POINT('Ctrl Pts',(13.50645002116,3.55687970080345,-10.4878133509968));
#30563=CARTESIAN_POINT('Ctrl Pts',(13.4877362194611,3.49520612255947,-10.5063727943728));
#30564=CARTESIAN_POINT('Ctrl Pts',(13.4695047273751,3.4333370053469,-10.5244681666954));
#30565=CARTESIAN_POINT('Ctrl Pts',(13.4517586041853,3.3712758922898,-10.5420943430048));
#30566=CARTESIAN_POINT('Ctrl Pts',(13.3622742346147,3.05833432655265,-10.6309738835175));
#30567=CARTESIAN_POINT('Ctrl Pts',(13.285027440584,2.74021475838435,-10.7080055004884));
#30568=CARTESIAN_POINT('Ctrl Pts',(13.2203229329071,2.41674037456619,-10.7726649043609));
#30569=CARTESIAN_POINT('Ctrl Pts',(13.2114517859957,2.37239124211817,-10.78152986743));
#30570=CARTESIAN_POINT('Ctrl Pts',(13.2028162317113,2.32794154603814,-10.790162469246));
#30571=CARTESIAN_POINT('Ctrl Pts',(13.1944181700145,2.28339038153381,-10.7985604911309));
#30572=CARTESIAN_POINT('Ctrl Pts',(13.1588819633499,2.09487314432792,-10.8340965293319));
#30573=CARTESIAN_POINT('Ctrl Pts',(13.1276141068245,1.90466457826725,-10.8654110680939));
#30574=CARTESIAN_POINT('Ctrl Pts',(13.1007158995053,1.71250392639037,-10.8923720428026));
#30575=CARTESIAN_POINT('Ctrl Pts',(13.078181338771,1.55151714280708,-10.9149591882885));
#30576=CARTESIAN_POINT('Ctrl Pts',(13.0587141602199,1.38916002469534,-10.9344902732969));
#30577=CARTESIAN_POINT('Ctrl Pts',(13.0423929369339,1.2252700508822,-10.950868868793));
#30578=CARTESIAN_POINT('Ctrl Pts',(13.0400111714759,1.20135349317773,-10.9532590066104));
#30579=CARTESIAN_POINT('Ctrl Pts',(13.0376990687219,1.17741998485909,-10.9555793246671));
#30580=CARTESIAN_POINT('Ctrl Pts',(13.0354566331901,1.15347096186712,-10.9578297968203));
#30581=CARTESIAN_POINT('Ctrl Pts',(13.0191094472756,0.978884390356729,-10.974235569099));
#30582=CARTESIAN_POINT('Ctrl Pts',(13.0064991064528,0.803827357803935,-10.9868998425679));
#30583=CARTESIAN_POINT('Ctrl Pts',(12.9975961675176,0.628791258833778,-10.9958441879377));
#30584=CARTESIAN_POINT('Ctrl Pts',(12.988664151061,0.453183481684936,-11.0048177460648));
#30585=CARTESIAN_POINT('Ctrl Pts',(12.9834637624987,0.27759563306974,-11.0100470817015));
#30586=CARTESIAN_POINT('Ctrl Pts',(12.9820016174814,0.102519509885962,-11.0115175695696));
#30587=CARTESIAN_POINT('Ctrl Pts',(12.98172134674,0.0689601062285234,-11.0117994395073));
#30588=CARTESIAN_POINT('Ctrl Pts',(12.9815785380294,0.0354195213508229,
-11.011943089827));
#30589=CARTESIAN_POINT('Ctrl Pts',(12.9815733914891,0.00190125514371761,
-11.0119482630768));
#30590=CARTESIAN_POINT('Ctrl Pts',(12.9815732941799,0.00126750194249285,
-11.011948360891));
#30591=CARTESIAN_POINT('Ctrl Pts',(12.9815732453836,0.000633750239677955,
-11.0119484099057));
#30592=CARTESIAN_POINT('Ctrl Pts',(12.9815732451008,2.5445788709682E-11,
-11.0119484101204));
#30593=CARTESIAN_POINT('Origin',(23.3621596556826,0.,0.));
#30594=CARTESIAN_POINT('',(32.3980051060631,6.53333333333333,-5.0726277758567));
#30595=CARTESIAN_POINT('Origin',(23.3621596556826,6.53333333333333,0.));
#30596=CARTESIAN_POINT('Ctrl Pts',(32.3980051060631,6.53333333333333,-5.0726277758567));
#30597=CARTESIAN_POINT('Ctrl Pts',(31.8794776108994,7.25152719230469,-5.07127432142549));
#30598=CARTESIAN_POINT('Ctrl Pts',(31.2870113030289,7.89449624331078,-5.06972733998685));
#30599=CARTESIAN_POINT('Ctrl Pts',(30.2913441883522,8.75012170898564,-5.06712608463878));
#30600=CARTESIAN_POINT('Ctrl Pts',(29.9397905959016,9.01808940429159,-5.06620740040415));
#30601=CARTESIAN_POINT('Ctrl Pts',(29.2064698119968,9.51076354319072,-5.06429050665035));
#30602=CARTESIAN_POINT('Ctrl Pts',(28.8285643445812,9.73317788561662,-5.06330239329255));
#30603=CARTESIAN_POINT('Ctrl Pts',(28.0509957610249,10.1317194379082,-5.0612686463517));
#30604=CARTESIAN_POINT('Ctrl Pts',(27.6513307809873,10.3078426825288,-5.06022300812922));
#30605=CARTESIAN_POINT('Ctrl Pts',(26.830050466374,10.6133920770874,-5.05807360020096));
#30606=CARTESIAN_POINT('Ctrl Pts',(26.4058705401804,10.7433739392376,-5.05696311341597));
#30607=CARTESIAN_POINT('Ctrl Pts',(25.1195669733215,11.0550325352827,-5.05359447050841));
#30608=CARTESIAN_POINT('Ctrl Pts',(24.247974768937,11.1600524072644,-5.05131040103342));
#30609=CARTESIAN_POINT('Ctrl Pts',(23.3621596985497,11.1611032573945,-5.04898743093873));
#30610=CARTESIAN_POINT('',(32.3980051060631,-6.53333333333333,-5.07262777585671));
#30611=CARTESIAN_POINT('Ctrl Pts',(23.3622216892987,-11.1611031836844,-5.04898759350387));
#30612=CARTESIAN_POINT('Ctrl Pts',(24.2480154606686,-11.1600475041801,-5.051310507669));
#30613=CARTESIAN_POINT('Ctrl Pts',(25.1195869910657,-11.0550276851818,-5.05359452293198));
#30614=CARTESIAN_POINT('Ctrl Pts',(26.4058705401804,-10.7433739392376,-5.05696311341597));
#30615=CARTESIAN_POINT('Ctrl Pts',(26.830050466374,-10.6133920770874,-5.05807360020097));
#30616=CARTESIAN_POINT('Ctrl Pts',(27.6513307809873,-10.3078426825288,-5.06022300812922));
#30617=CARTESIAN_POINT('Ctrl Pts',(28.0509957610249,-10.1317194379082,-5.0612686463517));
#30618=CARTESIAN_POINT('Ctrl Pts',(28.8285643445811,-9.73317788561662,-5.06330239329256));
#30619=CARTESIAN_POINT('Ctrl Pts',(29.2064698119968,-9.51076354319072,-5.06429050665035));
#30620=CARTESIAN_POINT('Ctrl Pts',(29.9397905959016,-9.01808940429159,-5.06620740040415));
#30621=CARTESIAN_POINT('Ctrl Pts',(30.2913441883522,-8.75012170898565,-5.06712608463878));
#30622=CARTESIAN_POINT('Ctrl Pts',(31.2870113030289,-7.89449624331078,-5.06972733998685));
#30623=CARTESIAN_POINT('Ctrl Pts',(31.8794776108994,-7.2515271923047,-5.07127432142564));
#30624=CARTESIAN_POINT('Ctrl Pts',(32.3980051060631,-6.53333333333333,-5.07262777585671));
#30625=CARTESIAN_POINT('Origin',(23.3621596556826,-6.53333333333334,0.));
#30626=CARTESIAN_POINT('Origin',(-60.4312629272455,0.,0.));
#30627=CARTESIAN_POINT('',(16.3099360798356,-6.,0.));
#30628=CARTESIAN_POINT('',(-60.4312629272455,-6.,0.));
#30629=CARTESIAN_POINT('',(14.1,4.89395944902277E-17,-6.));
#30630=CARTESIAN_POINT('Ctrl Pts',(16.3099360798356,-6.,6.93889390390723E-17));
#30631=CARTESIAN_POINT('Ctrl Pts',(16.3099360798356,-6.,-0.786255652352734));
#30632=CARTESIAN_POINT('Ctrl Pts',(16.1646223990385,-5.83790831484214,-1.59718008826893));
#30633=CARTESIAN_POINT('Ctrl Pts',(15.7042167515933,-5.22042193256505,-3.06257657270413));
#30634=CARTESIAN_POINT('Ctrl Pts',(15.3999322551341,-4.76490888973131,-3.72037248450726));
#30635=CARTESIAN_POINT('Ctrl Pts',(14.8633582506416,-3.72535685789928,-4.75992451633929));
#30636=CARTESIAN_POINT('Ctrl Pts',(14.5899394843239,-3.06638866080029,-5.21878459930749));
#30637=CARTESIAN_POINT('Ctrl Pts',(14.2066217507266,-1.59374871804443,-5.83938521356375));
#30638=CARTESIAN_POINT('Ctrl Pts',(14.1,-0.778751860750423,-6.));
#30639=CARTESIAN_POINT('Ctrl Pts',(14.1,6.93889390390723E-16,-6.));
#30640=CARTESIAN_POINT('',(-3.88784034431744,-7.34788079488412E-16,-6.));
#30641=CARTESIAN_POINT('',(-60.4312629272455,-7.34788079488412E-16,-6.));
#30642=CARTESIAN_POINT('Origin',(-3.88784034431744,0.,0.));
#30643=CARTESIAN_POINT('',(16.3099360798356,6.,0.));
#30644=CARTESIAN_POINT('Ctrl Pts',(14.1,6.93889390390723E-16,-6.));
#30645=CARTESIAN_POINT('Ctrl Pts',(14.1,0.778751860750424,-6.));
#30646=CARTESIAN_POINT('Ctrl Pts',(14.2066217507266,1.59374871804443,-5.83938521356375));
#30647=CARTESIAN_POINT('Ctrl Pts',(14.5899394843239,3.06638866080029,-5.21878459930749));
#30648=CARTESIAN_POINT('Ctrl Pts',(14.8633582506416,3.72535685789928,-4.75992451633929));
#30649=CARTESIAN_POINT('Ctrl Pts',(15.3999322551341,4.76490888973131,-3.72037248450726));
#30650=CARTESIAN_POINT('Ctrl Pts',(15.7042167515933,5.22042193256505,-3.06257657270413));
#30651=CARTESIAN_POINT('Ctrl Pts',(16.1646223990385,5.83790831484214,-1.59718008826893));
#30652=CARTESIAN_POINT('Ctrl Pts',(16.3099360798356,6.,-0.786255652352734));
#30653=CARTESIAN_POINT('Ctrl Pts',(16.3099360798356,6.,0.));
#30654=CARTESIAN_POINT('',(-60.4312629272455,6.,0.));
#30655=CARTESIAN_POINT('Origin',(-3.88784034431744,9.,0.));
#30656=CARTESIAN_POINT('Origin',(31.6603850692973,-6.,0.));
#30657=CARTESIAN_POINT('Origin',(23.35,0.,0.));
#30658=CARTESIAN_POINT('Origin',(31.6603850692973,-6.,0.));
#30659=CARTESIAN_POINT('Origin',(23.35,0.,0.));
#30660=CARTESIAN_POINT('Origin',(23.35,0.,-12.25));
#30661=CARTESIAN_POINT('',(29.8644600669621,-6.56691023510729,-0.418815697553272));
#30662=CARTESIAN_POINT('Ctrl Pts',(23.3560798277625,-9.24999837277875,-1.61173889512423E-9));
#30663=CARTESIAN_POINT('Ctrl Pts',(23.3557691145709,-9.24999837121855,-0.00598343755341071));
#30664=CARTESIAN_POINT('Ctrl Pts',(23.3585014101503,-9.24999612954719,-0.0105107270823176));
#30665=CARTESIAN_POINT('Ctrl Pts',(23.3624176778877,-9.24999071299229,-0.0142079838995739));
#30666=CARTESIAN_POINT('Ctrl Pts',(23.3653670356748,-9.2499866337619,-0.0169924036369621));
#30667=CARTESIAN_POINT('Ctrl Pts',(23.3689921278142,-9.24998075272328,-0.0193042883238705));
#30668=CARTESIAN_POINT('Ctrl Pts',(23.3724772454019,-9.24997260146442,-0.0214104444082658));
#30669=CARTESIAN_POINT('Ctrl Pts',(23.3726619716849,-9.24997216941249,-0.0215220797763884));
#30670=CARTESIAN_POINT('Ctrl Pts',(23.3728462918676,-9.24997173096435,-0.0216331397566146));
#30671=CARTESIAN_POINT('Ctrl Pts',(23.3730300796674,-9.24997128604387,-0.0217436651116202));
#30672=CARTESIAN_POINT('Ctrl Pts',(23.3734340225806,-9.24997030816355,-0.0219865862083058));
#30673=CARTESIAN_POINT('Ctrl Pts',(23.3738353945868,-9.24996929901756,-0.0222269243807324));
#30674=CARTESIAN_POINT('Ctrl Pts',(23.3742328222902,-9.24996825784747,-0.0224651013272281));
#30675=CARTESIAN_POINT('Ctrl Pts',(23.3801893417519,-9.24995265312272,-0.0260348213165618));
#30676=CARTESIAN_POINT('Ctrl Pts',(23.3865182047679,-9.24993006766998,-0.0290684294421575));
#30677=CARTESIAN_POINT('Ctrl Pts',(23.3930123216858,-9.24989993362502,-0.0318040938194547));
#30678=CARTESIAN_POINT('Ctrl Pts',(23.3949401747841,-9.24989098798812,-0.0326162071694723));
#30679=CARTESIAN_POINT('Ctrl Pts',(23.3968823886159,-9.2498813781345,-0.0334023642156201));
#30680=CARTESIAN_POINT('Ctrl Pts',(23.3988330813282,-9.24987109186398,-0.0341694944181134));
#30681=CARTESIAN_POINT('Ctrl Pts',(23.3994515849643,-9.24986783040939,-0.0344127274073939));
#30682=CARTESIAN_POINT('Ctrl Pts',(23.4000705048499,-9.24986450325595,-0.0346538603830449));
#30683=CARTESIAN_POINT('Ctrl Pts',(23.400689667918,-9.24986111021179,-0.0348931350363281));
#30684=CARTESIAN_POINT('Ctrl Pts',(23.4180099648753,-9.24976619412998,-0.0415865382167911));
#30685=CARTESIAN_POINT('Ctrl Pts',(23.4356558940743,-9.24962047407717,-0.0467247754339533));
#30686=CARTESIAN_POINT('Ctrl Pts',(23.4534448814473,-9.24942155576377,-0.0513789487715506));
#30687=CARTESIAN_POINT('Ctrl Pts',(23.454205883255,-9.24941304616214,-0.0515780514100856));
#30688=CARTESIAN_POINT('Ctrl Pts',(23.4549670822585,-9.24940443982341,-0.0517762560936749));
#30689=CARTESIAN_POINT('Ctrl Pts',(23.4557284619145,-9.24939573660621,-0.0519736470538049));
#30690=CARTESIAN_POINT('Ctrl Pts',(23.4918351889383,-9.24898300599922,-0.0613344717854022));
#30691=CARTESIAN_POINT('Ctrl Pts',(23.5284025808039,-9.24835241857728,-0.0685880793220111));
#30692=CARTESIAN_POINT('Ctrl Pts',(23.5651479404171,-9.24749757107013,-0.0751658425167519));
#30693=CARTESIAN_POINT('Ctrl Pts',(23.5660485062986,-9.24747662022064,-0.0753270522360871));
#30694=CARTESIAN_POINT('Ctrl Pts',(23.5669491575448,-9.2474555351634,-0.0754878537145558));
#30695=CARTESIAN_POINT('Ctrl Pts',(23.5678498899729,-9.24743431582261,-0.0756482682765296));
#30696=CARTESIAN_POINT('Ctrl Pts',(23.6420034473011,-9.24568741568394,-0.0888545324753748));
#30697=CARTESIAN_POINT('Ctrl Pts',(23.7165177601391,-9.24303700572992,-0.0990718482177321));
#30698=CARTESIAN_POINT('Ctrl Pts',(23.7910628709197,-9.23947853064399,-0.108338143439424));
#30699=CARTESIAN_POINT('Ctrl Pts',(23.7920741160351,-9.23943025798719,-0.108463845791768));
#30700=CARTESIAN_POINT('Ctrl Pts',(23.7930853619844,-9.23938181845271,-0.108589371555579));
#30701=CARTESIAN_POINT('Ctrl Pts',(23.7940966079193,-9.23933321203489,-0.10871472582196));
#30702=CARTESIAN_POINT('Ctrl Pts',(23.9439866829755,-9.23212861485126,-0.127295132177851));
#30703=CARTESIAN_POINT('Ctrl Pts',(24.094105898176,-9.22125394152026,-0.141687403613213));
#30704=CARTESIAN_POINT('Ctrl Pts',(24.2441262196889,-9.20668443566019,-0.154746477332881));
#30705=CARTESIAN_POINT('Ctrl Pts',(24.2451816356825,-9.2065819369497,-0.154838349921378));
#30706=CARTESIAN_POINT('Ctrl Pts',(24.2462370466876,-9.20647925543194,-0.154930156309389));
#30707=CARTESIAN_POINT('Ctrl Pts',(24.2472924526095,-9.20637639109876,-0.155021897491501));
#30708=CARTESIAN_POINT('Ctrl Pts',(24.5482990564597,-9.17703901204522,-0.181186902906664));
#30709=CARTESIAN_POINT('Ctrl Pts',(24.8468428326049,-9.13300625249746,-0.201286064954757));
#30710=CARTESIAN_POINT('Ctrl Pts',(25.1409132619702,-9.07497270906441,-0.219347970745817));
#30711=CARTESIAN_POINT('Ctrl Pts',(25.1418786391976,-9.07478219599115,-0.219407264543468));
#30712=CARTESIAN_POINT('Ctrl Pts',(25.1428439684873,-9.07459153201271,-0.219466536374313));
#30713=CARTESIAN_POINT('Ctrl Pts',(25.1438092497709,-9.07440071715349,-0.219525786380926));
#30714=CARTESIAN_POINT('Ctrl Pts',(25.6986244953389,-8.96472595730263,-0.253580944731915));
#30715=CARTESIAN_POINT('Ctrl Pts',(26.2398207194525,-8.80535458783623,-0.2798503572218));
#30716=CARTESIAN_POINT('Ctrl Pts',(26.7669586035649,-8.59575408308744,-0.303211664728421));
#30717=CARTESIAN_POINT('Ctrl Pts',(26.7996081847069,-8.58277196039532,-0.304658604756847));
#30718=CARTESIAN_POINT('Ctrl Pts',(26.8322038387004,-8.56959716131495,-0.306094393823134));
#30719=CARTESIAN_POINT('Ctrl Pts',(26.8647454628159,-8.55622956530362,-0.307520192718601));
#30720=CARTESIAN_POINT('Ctrl Pts',(26.8654093710352,-8.55595684207283,-0.307549281604956));
#30721=CARTESIAN_POINT('Ctrl Pts',(26.8660732568065,-8.55568403857651,-0.307578366327974));
#30722=CARTESIAN_POINT('Ctrl Pts',(26.8667371201291,-8.55541115481362,-0.307607446897494));
#30723=CARTESIAN_POINT('Ctrl Pts',(27.1454796620206,-8.44083288074899,-0.319817779345406));
#30724=CARTESIAN_POINT('Ctrl Pts',(27.4215277388667,-8.31121170489241,-0.331185606618138));
#30725=CARTESIAN_POINT('Ctrl Pts',(27.6880931473778,-8.16966632158923,-0.341697123203151));
#30726=CARTESIAN_POINT('Ctrl Pts',(27.6885803173162,-8.16940763590281,-0.341716333853613));
#30727=CARTESIAN_POINT('Ctrl Pts',(27.6890674556256,-8.16914891036779,-0.341735541645787));
#30728=CARTESIAN_POINT('Ctrl Pts',(27.6895545622644,-8.16889014500319,-0.341754746579587));
#30729=CARTESIAN_POINT('Ctrl Pts',(27.9562330077065,-8.02722271600935,-0.352268957396166));
#30730=CARTESIAN_POINT('Ctrl Pts',(28.2143884397778,-7.87337926937015,-0.361969675425041));
#30731=CARTESIAN_POINT('Ctrl Pts',(28.4641910486503,-7.70762933209229,-0.371041147542007));
#30732=CARTESIAN_POINT('Ctrl Pts',(28.4645007674479,-7.7074238263472,-0.371052394844221));
#30733=CARTESIAN_POINT('Ctrl Pts',(28.4648104733983,-7.70721830230421,-0.371063641178871));
#30734=CARTESIAN_POINT('Ctrl Pts',(28.4651201665019,-7.70701275996383,-0.371074886546309));
#30735=CARTESIAN_POINT('Ctrl Pts',(28.9095707576435,-7.41203229832873,-0.387213477126958));
#30736=CARTESIAN_POINT('Ctrl Pts',(29.327778597325,-7.07962587936707,-0.401386883213377));
#30737=CARTESIAN_POINT('Ctrl Pts',(29.7187223777706,-6.70836707619969,-0.414101709608085));
#30738=CARTESIAN_POINT('Ctrl Pts',(29.767730781015,-6.66182636614427,-0.415695630192842));
#30739=CARTESIAN_POINT('Ctrl Pts',(29.8163106926773,-6.61467503846194,-0.417266627326651));
#30740=CARTESIAN_POINT('Ctrl Pts',(29.8644600669621,-6.56691023510729,-0.418815697553251));
#30741=CARTESIAN_POINT('',(30.4989465761475,-5.86984351166102,-2.5869876306867));
#30742=CARTESIAN_POINT('Ctrl Pts',(29.8644600669621,-6.56691023510729,-0.418815697553272));
#30743=CARTESIAN_POINT('Ctrl Pts',(29.8733746637293,-6.55806683957206,-0.419102499544775));
#30744=CARTESIAN_POINT('Ctrl Pts',(29.8810061889829,-6.55046075135664,-0.426908455290693));
#30745=CARTESIAN_POINT('Ctrl Pts',(29.8934944746253,-6.53798577209718,-0.444265632584569));
#30746=CARTESIAN_POINT('Ctrl Pts',(29.8987214649284,-6.53274778761039,-0.454306399100273));
#30747=CARTESIAN_POINT('Ctrl Pts',(29.9131557521886,-6.51825686050047,-0.485213053623094));
#30748=CARTESIAN_POINT('Ctrl Pts',(29.9211884729116,-6.51015350884117,-0.507262215490086));
#30749=CARTESIAN_POINT('Ctrl Pts',(29.9439661829232,-6.48710849294812,-0.574043018301807));
#30750=CARTESIAN_POINT('Ctrl Pts',(29.9572126448329,-6.47360662755049,-0.619820775336012));
#30751=CARTESIAN_POINT('Ctrl Pts',(29.9959438791152,-6.43391768402986,-0.757554586253613));
#30752=CARTESIAN_POINT('Ctrl Pts',(30.0200501387962,-6.40891263751482,-0.850295961307722));
#30753=CARTESIAN_POINT('Ctrl Pts',(30.0926610277737,-6.33276736205838,-1.12809260388518));
#30754=CARTESIAN_POINT('Ctrl Pts',(30.1409280530889,-6.28101981664688,-1.31302684036839));
#30755=CARTESIAN_POINT('Ctrl Pts',(30.2895149536044,-6.11778450470958,-1.86433248511176));
#30756=CARTESIAN_POINT('Ctrl Pts',(30.3930163475332,-5.99885709501432,-2.22754310454855));
#30757=CARTESIAN_POINT('Ctrl Pts',(30.4989465761475,-5.86984351166102,-2.5869876306867));
#30758=CARTESIAN_POINT('',(30.8496157942439,-5.41463414634147,-3.60555127546399));
#30759=CARTESIAN_POINT('Ctrl Pts',(30.4989465761475,-5.86984351166102,-2.5869876306867));
#30760=CARTESIAN_POINT('Ctrl Pts',(30.5547782956591,-5.80184545017096,-2.7764369102171));
#30761=CARTESIAN_POINT('Ctrl Pts',(30.6146971569704,-5.72690380650632,-2.96137640232734));
#30762=CARTESIAN_POINT('Ctrl Pts',(30.677808767019,-5.64497703242559,-3.14209440617126));
#30763=CARTESIAN_POINT('Ctrl Pts',(30.7328569315897,-5.57351762045888,-3.29972300111334));
#30764=CARTESIAN_POINT('Ctrl Pts',(30.7903333826036,-5.49674409110279,-3.45414026184368));
#30765=CARTESIAN_POINT('Ctrl Pts',(30.8496157942439,-5.41463414634147,-3.60555127546398));
#30766=CARTESIAN_POINT('',(30.8496157942439,-5.41463414634147,-4.65853571252147));
#30767=CARTESIAN_POINT('',(30.8496157942439,-5.41463414634147,-12.25));
#30768=CARTESIAN_POINT('',(23.4134558714741,-9.24978690988232,-4.63699261464813));
#30769=CARTESIAN_POINT('Ctrl Pts',(30.8496157942439,-5.41463414634147,-4.65853571252147));
#30770=CARTESIAN_POINT('Ctrl Pts',(30.4224818233768,-6.00624210868884,-4.65730028266087));
#30771=CARTESIAN_POINT('Ctrl Pts',(29.9348006057638,-6.5362496484837,-4.65588924421514));
#30772=CARTESIAN_POINT('Ctrl Pts',(29.1157096677008,-7.24216864268045,-4.65351797766776));
#30773=CARTESIAN_POINT('Ctrl Pts',(28.8267164809711,-7.46328115931847,-4.65268114057206));
#30774=CARTESIAN_POINT('Ctrl Pts',(28.2233249304723,-7.87055863316035,-4.65093338408782));
#30775=CARTESIAN_POINT('Ctrl Pts',(27.9124127490458,-8.05459039487177,-4.65003256384235));
#30776=CARTESIAN_POINT('Ctrl Pts',(27.2727683495141,-8.38474358569576,-4.64817872235552));
#30777=CARTESIAN_POINT('Ctrl Pts',(26.9440345067492,-8.53086155850978,-4.6472256966148));
#30778=CARTESIAN_POINT('Ctrl Pts',(26.2686099494916,-8.78489606818956,-4.64526695104862));
#30779=CARTESIAN_POINT('Ctrl Pts',(25.9199435996119,-8.89326151785136,-4.64425549764083));
#30780=CARTESIAN_POINT('Ctrl Pts',(24.8609128854777,-9.15469739384237,-4.64118229168174));
#30781=CARTESIAN_POINT('Ctrl Pts',(24.1431288109746,-9.24477620324171,-4.63909799546489));
#30782=CARTESIAN_POINT('Ctrl Pts',(23.4134608743401,-9.24978230648852,-4.63697771328011));
#30783=CARTESIAN_POINT('',(23.4134609280924,9.249790502254,-4.63697771320315));
#30784=CARTESIAN_POINT('Ctrl Pts',(23.4134536511895,-9.24977205774196,-4.63699888793905));
#30785=CARTESIAN_POINT('Ctrl Pts',(23.3625154232152,-9.25012518184601,-4.6198065222011));
#30786=CARTESIAN_POINT('Ctrl Pts',(23.3113786668813,-9.25006107462989,-4.6034901913981));
#30787=CARTESIAN_POINT('Ctrl Pts',(23.2601805794695,-9.24956390714826,-4.58816205258291));
#30788=CARTESIAN_POINT('Ctrl Pts',(23.0981361101497,-9.24799034757217,-4.53964773797597));
#30789=CARTESIAN_POINT('Ctrl Pts',(22.9348134041621,-9.24215350764586,-4.50067157209841));
#30790=CARTESIAN_POINT('Ctrl Pts',(22.7699677329688,-9.23179628076355,-4.47253333001147));
#30791=CARTESIAN_POINT('Ctrl Pts',(22.6606958452985,-9.22493074571938,-4.45388122464344));
#30792=CARTESIAN_POINT('Ctrl Pts',(22.5507538239542,-9.21607845109921,-4.43999863426792));
#30793=CARTESIAN_POINT('Ctrl Pts',(22.4400833769471,-9.20513819700547,-4.43119193287283));
#30794=CARTESIAN_POINT('Ctrl Pts',(22.3843570454958,-9.19962940724021,-4.42675745940491));
#30795=CARTESIAN_POINT('Ctrl Pts',(22.3283580105308,-9.1935818903447,-4.42360382581514));
#30796=CARTESIAN_POINT('Ctrl Pts',(22.2721719172255,-9.18699007422903,-4.42178202558678));
#30797=CARTESIAN_POINT('Ctrl Pts',(22.1990930360943,-9.17841637710902,-4.41941248688955));
#30798=CARTESIAN_POINT('Ctrl Pts',(22.1257309771798,-9.16890595979547,-4.41934771320976));
#30799=CARTESIAN_POINT('Ctrl Pts',(22.0527227559231,-9.15856206490708,-4.42150072981427));
#30800=CARTESIAN_POINT('Ctrl Pts',(22.0154729646368,-9.153284468507,-4.42259922828161));
#30801=CARTESIAN_POINT('Ctrl Pts',(21.9783152749303,-9.14779021638894,-4.42427425890002));
#30802=CARTESIAN_POINT('Ctrl Pts',(21.9413331248964,-9.14209478477932,-4.42650949742667));
#30803=CARTESIAN_POINT('Ctrl Pts',(21.8845228329765,-9.13334572254104,-4.42994316888961));
#30804=CARTESIAN_POINT('Ctrl Pts',(21.8279757871699,-9.12409883599493,-4.43470752363319));
#30805=CARTESIAN_POINT('Ctrl Pts',(21.7719128739377,-9.11439197218095,-4.4407627349337));
#30806=CARTESIAN_POINT('Ctrl Pts',(21.6649547696481,-9.09587299604709,-4.45231500513226));
#30807=CARTESIAN_POINT('Ctrl Pts',(21.5591625981775,-9.0756190286987,-4.46851612585592));
#30808=CARTESIAN_POINT('Ctrl Pts',(21.454548075228,-9.0537166137703,-4.48890446567054));
#30809=CARTESIAN_POINT('Ctrl Pts',(21.3980429074417,-9.041886519864,-4.49991676615835));
#30810=CARTESIAN_POINT('Ctrl Pts',(21.3418595080924,-9.02957122376613,-4.51215442073769));
#30811=CARTESIAN_POINT('Ctrl Pts',(21.2859920296565,-9.01678274654428,-4.52554647006272));
#30812=CARTESIAN_POINT('Ctrl Pts',(21.1261165989934,-8.98018608314352,-4.56387036999955));
#30813=CARTESIAN_POINT('Ctrl Pts',(20.968827586669,-8.93971141831164,-4.61163882662143));
#30814=CARTESIAN_POINT('Ctrl Pts',(20.8139926873238,-8.89557007225076,-4.66712904960507));
#30815=CARTESIAN_POINT('Ctrl Pts',(20.7175752575018,-8.8680827605783,-4.70168343432688));
#30816=CARTESIAN_POINT('Ctrl Pts',(20.6227601556529,-8.83935856288174,-4.73899129256353));
#30817=CARTESIAN_POINT('Ctrl Pts',(20.5295418854412,-8.80951347275127,-4.77853066159051));
#30818=CARTESIAN_POINT('Ctrl Pts',(20.4722797482889,-8.79118022498244,-4.80281891288497));
#30819=CARTESIAN_POINT('Ctrl Pts',(20.415594740856,-8.77241599294277,-4.82796055678945));
#30820=CARTESIAN_POINT('Ctrl Pts',(20.3594786464077,-8.75324408626673,-4.85384151791365));
#30821=CARTESIAN_POINT('Ctrl Pts',(20.2112845228144,-8.70261397853378,-4.9221892243829));
#30822=CARTESIAN_POINT('Ctrl Pts',(20.0668379773865,-8.64907446285856,-4.99577768538368));
#30823=CARTESIAN_POINT('Ctrl Pts',(19.9255222376653,-8.59275578941024,-5.07319877354532));
#30824=CARTESIAN_POINT('Ctrl Pts',(19.8444601752456,-8.56045006160199,-5.11760934729691));
#30825=CARTESIAN_POINT('Ctrl Pts',(19.7643251743023,-8.52718104617017,-5.16333201725847));
#30826=CARTESIAN_POINT('Ctrl Pts',(19.6851507542395,-8.49301403080143,-5.21011167025964));
#30827=CARTESIAN_POINT('Ctrl Pts',(19.5204367414571,-8.42193316653096,-5.30743179406061));
#30828=CARTESIAN_POINT('Ctrl Pts',(19.3594003020667,-8.34675420139556,-5.40956187554908));
#30829=CARTESIAN_POINT('Ctrl Pts',(19.2025571830132,-8.26808276251442,-5.51423100984347));
#30830=CARTESIAN_POINT('Ctrl Pts',(19.1705496927634,-8.25202802368925,-5.53559118372682));
#30831=CARTESIAN_POINT('Ctrl Pts',(19.1387167227146,-8.2358279579899,-5.55705704428414));
#30832=CARTESIAN_POINT('Ctrl Pts',(19.1070624667525,-8.21948788514045,-5.57860925559438));
#30833=CARTESIAN_POINT('Ctrl Pts',(19.040072240914,-8.1849072217468,-5.62422042095298));
#30834=CARTESIAN_POINT('Ctrl Pts',(18.973874871607,-8.14970640323712,-5.67021831303887));
#30835=CARTESIAN_POINT('Ctrl Pts',(18.9084396350559,-8.11389278588748,-5.71652425076615));
#30836=CARTESIAN_POINT('Ctrl Pts',(18.7176376007028,-8.00946417207001,-5.85154732986952));
#30837=CARTESIAN_POINT('Ctrl Pts',(18.5329968378859,-7.89965487887584,-5.98927781427906));
#30838=CARTESIAN_POINT('Ctrl Pts',(18.3533564211586,-7.78434666162082,-6.12812846959049));
#30839=CARTESIAN_POINT('Ctrl Pts',(18.2996301970183,-7.74986068547852,-6.16965543532115));
#30840=CARTESIAN_POINT('Ctrl Pts',(18.2463541938633,-7.71488252716231,-6.2112866342043));
#30841=CARTESIAN_POINT('Ctrl Pts',(18.1935123904376,-7.67940451382411,-6.25299729234993));
#30842=CARTESIAN_POINT('Ctrl Pts',(18.0087538346775,-7.55535752676715,-6.39883639054874));
#30843=CARTESIAN_POINT('Ctrl Pts',(17.8292147797447,-7.42513966469565,-6.54564052692412));
#30844=CARTESIAN_POINT('Ctrl Pts',(17.6543191662457,-7.28846484833837,-6.69218578884888));
#30845=CARTESIAN_POINT('Ctrl Pts',(17.4293790572173,-7.11268200577425,-6.88066339863838));
#30846=CARTESIAN_POINT('Ctrl Pts',(17.2121426350658,-6.92622255174211,-7.0687519212596));
#30847=CARTESIAN_POINT('Ctrl Pts',(17.0021480411652,-6.72809597948268,-7.25458119189773));
#30848=CARTESIAN_POINT('Ctrl Pts',(16.9697452200666,-6.69752443115584,-7.28325522821234));
#30849=CARTESIAN_POINT('Ctrl Pts',(16.9374967681784,-6.66665407851879,-7.3118928664918));
#30850=CARTESIAN_POINT('Ctrl Pts',(16.9054125928198,-6.63549059697695,-7.34047940783783));
#30851=CARTESIAN_POINT('Ctrl Pts',(16.7671279762097,-6.50117422296744,-7.463689023359));
#30852=CARTESIAN_POINT('Ctrl Pts',(16.6316353181641,-6.36115478230237,-7.58616693585297));
#30853=CARTESIAN_POINT('Ctrl Pts',(16.4998949000094,-6.21598638326824,-7.70660105121202));
#30854=CARTESIAN_POINT('Ctrl Pts',(16.4643815647232,-6.17685325996352,-7.73906654038045));
#30855=CARTESIAN_POINT('Ctrl Pts',(16.4291407972998,-6.137346246477,-7.77138348493443));
#30856=CARTESIAN_POINT('Ctrl Pts',(16.3941911402224,-6.09747678193591,-7.80352619206129));
#30857=CARTESIAN_POINT('Ctrl Pts',(16.3704901831911,-6.07043947899866,-7.82532362826506));
#30858=CARTESIAN_POINT('Ctrl Pts',(16.346936709246,-6.04325350110009,-7.84702809310363));
#30859=CARTESIAN_POINT('Ctrl Pts',(16.3235317154403,-6.01591845087238,-7.86863650241515));
#30860=CARTESIAN_POINT('Ctrl Pts',(16.1552502807965,-5.81937998961162,-8.02400053068656));
#30861=CARTESIAN_POINT('Ctrl Pts',(15.9944684313001,-5.6149337711535,-8.17456347625085));
#30862=CARTESIAN_POINT('Ctrl Pts',(15.8412586152749,-5.40197212305963,-8.31941227715205));
#30863=CARTESIAN_POINT('Ctrl Pts',(15.8251737266489,-5.3796141274685,-8.33461937608707));
#30864=CARTESIAN_POINT('Ctrl Pts',(15.8091710738808,-5.35716349022867,-8.34976430237018));
#30865=CARTESIAN_POINT('Ctrl Pts',(15.7932513756019,-5.33461898106988,-8.36484577448847));
#30866=CARTESIAN_POINT('Ctrl Pts',(15.6711357265184,-5.16168622060058,-8.48053162007448));
#30867=CARTESIAN_POINT('Ctrl Pts',(15.5539386693611,-4.98328907382023,-8.59246306301524));
#30868=CARTESIAN_POINT('Ctrl Pts',(15.4419436637423,-4.7988015802883,-8.70010725775847));
#30869=CARTESIAN_POINT('Ctrl Pts',(15.3349318152216,-4.62252275782897,-8.80296188237635));
#30870=CARTESIAN_POINT('Ctrl Pts',(15.2326693884291,-4.44068357906781,-8.90190244898871));
#30871=CARTESIAN_POINT('Ctrl Pts',(15.135429249196,-4.25270849650674,-8.99643824681075));
#30872=CARTESIAN_POINT('Ctrl Pts',(15.0615819586205,-4.10995417044033,-9.06823177350253));
#30873=CARTESIAN_POINT('Ctrl Pts',(14.9906316960674,-3.96366048599508,-9.13748442942233));
#30874=CARTESIAN_POINT('Ctrl Pts',(14.9227086452196,-3.81356269417404,-9.20396968784947));
#30875=CARTESIAN_POINT('Ctrl Pts',(14.9168048317238,-3.80051632246408,-9.20974852965753));
#30876=CARTESIAN_POINT('Ctrl Pts',(14.9109288888533,-3.78745181862973,-9.2155015917612));
#30877=CARTESIAN_POINT('Ctrl Pts',(14.9050809147943,-3.77436910755354,-9.2212287385584));
#30878=CARTESIAN_POINT('Ctrl Pts',(14.8094865402887,-3.56051152721262,-9.31484800058859));
#30879=CARTESIAN_POINT('Ctrl Pts',(14.7215332654277,-3.34217122454843,-9.40138352891765));
#30880=CARTESIAN_POINT('Ctrl Pts',(14.6415966822654,-3.11908192459304,-9.48029264021483));
#30881=CARTESIAN_POINT('Ctrl Pts',(14.5642383968141,-2.90318821154769,-9.55665659417615));
#30882=CARTESIAN_POINT('Ctrl Pts',(14.4943879619239,-2.68284690098548,-9.62587828797752));
#30883=CARTESIAN_POINT('Ctrl Pts',(14.432417365367,-2.45780017141991,-9.68743324706195));
#30884=CARTESIAN_POINT('Ctrl Pts',(14.3893243216042,-2.30130742962521,-9.73023726530642));
#30885=CARTESIAN_POINT('Ctrl Pts',(14.350042231419,-2.14253903782754,-9.76933335602689));
#30886=CARTESIAN_POINT('Ctrl Pts',(14.3147058328292,-1.98140336961855,-9.8045348690398));
#30887=CARTESIAN_POINT('Ctrl Pts',(14.3136044543346,-1.97638103098872,-9.80563204336872));
#30888=CARTESIAN_POINT('Ctrl Pts',(14.31250696286,-1.97135599428855,-9.80672539075607));
#30889=CARTESIAN_POINT('Ctrl Pts',(14.3114133683192,-1.96632830061353,-9.80781490049638));
#30890=CARTESIAN_POINT('Ctrl Pts',(14.2745987957367,-1.79707691281701,-9.844491963079));
#30891=CARTESIAN_POINT('Ctrl Pts',(14.2421976357723,-1.62478683090103,-9.87681844509401));
#30892=CARTESIAN_POINT('Ctrl Pts',(14.2146208502178,-1.45124442493548,-9.90435663415071));
#30893=CARTESIAN_POINT('Ctrl Pts',(14.1905893369956,-1.30001263559869,-9.92835451284191));
#30894=CARTESIAN_POINT('Ctrl Pts',(14.1702212471377,-1.14783143755459,-9.94871632506298));
#30895=CARTESIAN_POINT('Ctrl Pts',(14.1537676058962,-0.995896457287379,
-9.9651728621265));
#30896=CARTESIAN_POINT('Ctrl Pts',(14.1535154766557,-0.993568264358871,
-9.9654250357415));
#30897=CARTESIAN_POINT('Ctrl Pts',(14.1532642330707,-0.991240013867564,
-9.96567632576613));
#30898=CARTESIAN_POINT('Ctrl Pts',(14.1530138752056,-0.988911706202816,
-9.96592673211944));
#30899=CARTESIAN_POINT('Ctrl Pts',(14.1176771446479,-0.660283002753475,
-10.0012703065398));
#30900=CARTESIAN_POINT('Ctrl Pts',(14.0999586550532,-0.330265416703061,
-10.0190270165079));
#30901=CARTESIAN_POINT('Ctrl Pts',(14.1000000720546,0.00115476959212982,
-10.0189855634338));
#30902=CARTESIAN_POINT('Ctrl Pts',(14.1000000889788,0.00129019738339432,
-10.0189855464949));
#30903=CARTESIAN_POINT('Ctrl Pts',(14.1000001088685,0.00142562543411628,
-10.0189855265846));
#30904=CARTESIAN_POINT('Ctrl Pts',(14.1000001317237,0.00156105374426756,
-10.0189855037028));
#30905=CARTESIAN_POINT('Ctrl Pts',(14.1000358072751,0.212955982700576,-10.0189497867261));
#30906=CARTESIAN_POINT('Ctrl Pts',(14.1074048420233,0.425862245288223,-10.0115660274281));
#30907=CARTESIAN_POINT('Ctrl Pts',(14.122083690801,0.638308793476026,-9.99687450483632));
#30908=CARTESIAN_POINT('Ctrl Pts',(14.1304086932907,0.758796310539954,-9.98854231448503));
#30909=CARTESIAN_POINT('Ctrl Pts',(14.1410842316643,0.879135733516061,-9.97786025043846));
#30910=CARTESIAN_POINT('Ctrl Pts',(14.1541007419723,0.998967596774582,-9.96484091674184));
#30911=CARTESIAN_POINT('Ctrl Pts',(14.1543587496805,1.00134285279034,-9.9645828530696));
#30912=CARTESIAN_POINT('Ctrl Pts',(14.1546176737308,1.00371787914823,-9.96432387482324));
#30913=CARTESIAN_POINT('Ctrl Pts',(14.1548775139933,1.00609267334345,-9.96406398215856));
#30914=CARTESIAN_POINT('Ctrl Pts',(14.1811166565157,1.24590371242471,-9.937819547971));
#30915=CARTESIAN_POINT('Ctrl Pts',(14.2163411509945,1.48142568176268,-9.90260913254167));
#30916=CARTESIAN_POINT('Ctrl Pts',(14.2599907469931,1.71300461953484,-9.85906875646823));
#30917=CARTESIAN_POINT('Ctrl Pts',(14.2761915859853,1.79895668848331,-9.84290845518043));
#30918=CARTESIAN_POINT('Ctrl Pts',(14.2935533937762,1.88436542320633,-9.82560027869732));
#30919=CARTESIAN_POINT('Ctrl Pts',(14.3120487231286,1.96924799329246,-9.80717550881918));
#30920=CARTESIAN_POINT('Ctrl Pts',(14.313179333629,1.97443682357576,-9.80604921158513));
#30921=CARTESIAN_POINT('Ctrl Pts',(14.3143141770252,1.97962367355132,-9.80491874382379));
#30922=CARTESIAN_POINT('Ctrl Pts',(14.3154532468789,1.98480854635299,-9.8037841128692));
#30923=CARTESIAN_POINT('Ctrl Pts',(14.3836494945956,2.29522749810616,-9.73585362257075));
#30924=CARTESIAN_POINT('Ctrl Pts',(14.4670033588811,2.59855545823469,-9.6529906171091));
#30925=CARTESIAN_POINT('Ctrl Pts',(14.5647724800604,2.89521670871526,-9.55625712062353));
#30926=CARTESIAN_POINT('Ctrl Pts',(14.5677239339626,2.90417231754967,-9.5533369301561));
#30927=CARTESIAN_POINT('Ctrl Pts',(14.5706885923883,2.91312204824748,-9.55040404547431));
#30928=CARTESIAN_POINT('Ctrl Pts',(14.5736664294657,2.92206588883981,-9.5474584999236));
#30929=CARTESIAN_POINT('Ctrl Pts',(14.6311104426171,3.09459718698157,-9.4906374069767));
#30930=CARTESIAN_POINT('Ctrl Pts',(14.6937223783733,3.26537270008771,-9.42884780434795));
#30931=CARTESIAN_POINT('Ctrl Pts',(14.7605830856977,3.4327015772179,-9.36307478257347));
#30932=CARTESIAN_POINT('Ctrl Pts',(14.8069875664328,3.54883570091995,-9.31742520685158));
#30933=CARTESIAN_POINT('Ctrl Pts',(14.8554380267574,3.66331003509001,-9.26985741257131));
#30934=CARTESIAN_POINT('Ctrl Pts',(14.9056220961044,3.77557290469752,-9.22070457934102));
#30935=CARTESIAN_POINT('Ctrl Pts',(14.9115531749302,3.78884085880157,-9.21489537868846));
#30936=CARTESIAN_POINT('Ctrl Pts',(14.9175089427579,3.80207900624528,-9.20906364098573));
#30937=CARTESIAN_POINT('Ctrl Pts',(14.9234889314797,3.8152865178915,-9.2032098747074));
#30938=CARTESIAN_POINT('Ctrl Pts',(15.0533909246116,4.10219041804352,-9.07604978423608));
#30939=CARTESIAN_POINT('Ctrl Pts',(15.1950267960996,4.37660230577789,-8.9381228709984));
#30940=CARTESIAN_POINT('Ctrl Pts',(15.3475682128899,4.63969858186413,-8.79097067465315));
#30941=CARTESIAN_POINT('Ctrl Pts',(15.4869290652399,4.88006163903903,-8.65653337926571));
#30942=CARTESIAN_POINT('Ctrl Pts',(15.6353925190135,5.11097971039312,-8.5143956859272));
#30943=CARTESIAN_POINT('Ctrl Pts',(15.7923412757554,5.33332861190327,-8.36570498428764));
#30944=CARTESIAN_POINT('Ctrl Pts',(15.8085748204292,5.35632663304574,-8.35032558786711));
#30945=CARTESIAN_POINT('Ctrl Pts',(15.8249007586485,5.37923523180617,-8.33487457054184));
#30946=CARTESIAN_POINT('Ctrl Pts',(15.841318190271,5.40205493130655,-8.3193533874901));
#30947=CARTESIAN_POINT('Ctrl Pts',(15.9564445782044,5.56207689074639,-8.21051189618467));
#30948=CARTESIAN_POINT('Ctrl Pts',(16.0764315943577,5.7179387366289,-8.09791750495548));
#30949=CARTESIAN_POINT('Ctrl Pts',(16.199859969054,5.86835059952874,-7.98321179303217));
#30950=CARTESIAN_POINT('Ctrl Pts',(16.2413376889731,5.91889603640444,-7.94466529670187));
#30951=CARTESIAN_POINT('Ctrl Pts',(16.2832039606803,5.96882642578861,-7.90588033707161));
#30952=CARTESIAN_POINT('Ctrl Pts',(16.3254048483401,6.01809418238744,-7.86691892834382));
#30953=CARTESIAN_POINT('Ctrl Pts',(16.3490689997507,6.04572108116765,-7.84507131502498));
#30954=CARTESIAN_POINT('Ctrl Pts',(16.3728474309111,6.07315021492223,-7.82316039810069));
#30955=CARTESIAN_POINT('Ctrl Pts',(16.3967310211233,6.10037298103729,-7.80119685223178));
#30956=CARTESIAN_POINT('Ctrl Pts',(16.5406119366081,6.26436995451789,-7.66888277973158));
#30957=CARTESIAN_POINT('Ctrl Pts',(16.6887165728628,6.42152235603342,-7.53425782398027));
#30958=CARTESIAN_POINT('Ctrl Pts',(16.8408982921417,6.5722306611734,-7.39807639652365));
#30959=CARTESIAN_POINT('Ctrl Pts',(16.8616786155221,6.59280979072818,-7.3794809034884));
#30960=CARTESIAN_POINT('Ctrl Pts',(16.8825349128291,6.61326882820459,-7.36085640205674));
#30961=CARTESIAN_POINT('Ctrl Pts',(16.9034667668706,6.63360885105693,-7.34220482308772));
#30962=CARTESIAN_POINT('Ctrl Pts',(16.9356171064303,6.66485016585206,-7.3135568783815));
#30963=CARTESIAN_POINT('Ctrl Pts',(16.9679485682156,6.69581350788118,-7.28484298464478));
#30964=CARTESIAN_POINT('Ctrl Pts',(17.0004614301616,6.72650428901826,-7.25606858825597));
#30965=CARTESIAN_POINT('Ctrl Pts',(17.196485101874,6.91154243226739,-7.08258454244043));
#30966=CARTESIAN_POINT('Ctrl Pts',(17.3990929751407,7.08666865088716,-6.90688154140969));
#30967=CARTESIAN_POINT('Ctrl Pts',(17.6088306131168,7.25268813035639,-6.7303865509183));
#30968=CARTESIAN_POINT('Ctrl Pts',(17.6227451945787,7.26370232691938,-6.71867737965797));
#30969=CARTESIAN_POINT('Ctrl Pts',(17.6366911658378,7.27467642584925,-6.70696471709683));
#30970=CARTESIAN_POINT('Ctrl Pts',(17.6506686901954,7.28561065581231,-6.69524897787459));
#30971=CARTESIAN_POINT('Ctrl Pts',(17.8251083620105,7.42206997704129,-6.54903641170733));
#30972=CARTESIAN_POINT('Ctrl Pts',(18.0044456079559,7.55231948063633,-6.40232005328148));
#30973=CARTESIAN_POINT('Ctrl Pts',(18.1893889970805,7.67663444272538,-6.25626363447874));
#30974=CARTESIAN_POINT('Ctrl Pts',(18.2427346090674,7.7124922139231,-6.21413469392824));
#30975=CARTESIAN_POINT('Ctrl Pts',(18.2965462682594,7.74785583569029,-6.1720651548733));
#30976=CARTESIAN_POINT('Ctrl Pts',(18.3508438446585,7.78273330775818,-6.13008043092315));
#30977=CARTESIAN_POINT('Ctrl Pts',(18.5142781265021,7.88771358455781,-6.0037075122362));
#30978=CARTESIAN_POINT('Ctrl Pts',(18.6826314570586,7.98854931917481,-5.87771460460918));
#30979=CARTESIAN_POINT('Ctrl Pts',(18.8553464773727,8.08457873025275,-5.7543318478112));
#30980=CARTESIAN_POINT('Ctrl Pts',(18.9386356116647,8.13088742130181,-5.69483243090129));
#30981=CARTESIAN_POINT('Ctrl Pts',(19.0229393625003,8.176077953008,-5.63594037502953));
#30982=CARTESIAN_POINT('Ctrl Pts',(19.1081966589314,8.22007326509797,-5.57790904883187));
#30983=CARTESIAN_POINT('Ctrl Pts',(19.260373168651,8.2986008905112,-5.47432841650077));
#30984=CARTESIAN_POINT('Ctrl Pts',(19.4156079486,8.37340788319211,-5.37338156945517));
#30985=CARTESIAN_POINT('Ctrl Pts',(19.5746527036711,8.44450649480009,-5.27643569385595));
#30986=CARTESIAN_POINT('Ctrl Pts',(19.6098993308259,8.46026297952948,-5.2549510801074));
#30987=CARTESIAN_POINT('Ctrl Pts',(19.6453331883326,8.4758372773732,-5.23366312269295));
#30988=CARTESIAN_POINT('Ctrl Pts',(19.6809626607781,8.49122942455084,-5.21258698920787));
#30989=CARTESIAN_POINT('Ctrl Pts',(19.7602474117224,8.52548091556979,-5.16568716500225));
#30990=CARTESIAN_POINT('Ctrl Pts',(19.84051379949,8.5588361256642,-5.11984028725031));
#30991=CARTESIAN_POINT('Ctrl Pts',(19.9218515401125,8.59129199482057,-5.0752193141543));
#30992=CARTESIAN_POINT('Ctrl Pts',(20.0625119818507,8.64741916109783,-4.99805457195169));
#30993=CARTESIAN_POINT('Ctrl Pts',(20.2064041971235,8.70084633312459,-4.92460712543744));
#30994=CARTESIAN_POINT('Ctrl Pts',(20.3542553451009,8.75145781928091,-4.85625190593564));
#30995=CARTESIAN_POINT('Ctrl Pts',(20.4095323426498,8.77037989756356,-4.83069599140576));
#30996=CARTESIAN_POINT('Ctrl Pts',(20.4654213730509,8.78892550132495,-4.80583004620885));
#30997=CARTESIAN_POINT('Ctrl Pts',(20.521903888801,8.80706270078843,-4.78177653697074));
#30998=CARTESIAN_POINT('Ctrl Pts',(20.6157677318787,8.83720348367853,-4.74180390496927));
#30999=CARTESIAN_POINT('Ctrl Pts',(20.7113661107907,8.86624663007563,-4.70403416052498));
#31000=CARTESIAN_POINT('Ctrl Pts',(20.8085605831725,8.89401965877196,-4.66907541654005));
#31001=CARTESIAN_POINT('Ctrl Pts',(20.9633493392486,8.93825008113056,-4.61340125768304));
#31002=CARTESIAN_POINT('Ctrl Pts',(21.1207753957801,8.97886804824034,-4.56536356405399));
#31003=CARTESIAN_POINT('Ctrl Pts',(21.2809696644016,9.01563161793901,-4.5267531020893));
#31004=CARTESIAN_POINT('Ctrl Pts',(21.336234501468,9.02831454790188,-4.51343301949271));
#31005=CARTESIAN_POINT('Ctrl Pts',(21.3918288587508,9.04053919558814,-4.50123584390736));
#31006=CARTESIAN_POINT('Ctrl Pts',(21.4477584918535,9.05229263672872,-4.49023354869004));
#31007=CARTESIAN_POINT('Ctrl Pts',(21.5532816474144,9.07446800475902,-4.46947537729971));
#31008=CARTESIAN_POINT('Ctrl Pts',(21.6601522838149,9.09499736369338,-4.45294294540509));
#31009=CARTESIAN_POINT('Ctrl Pts',(21.7683635816266,9.11377672757539,-4.44114927475493));
#31010=CARTESIAN_POINT('Ctrl Pts',(21.8810210295216,9.1333276917614,-4.42887102965826));
#31011=CARTESIAN_POINT('Ctrl Pts',(21.9955129281085,9.15099632977271,-4.42182667462028));
#31012=CARTESIAN_POINT('Ctrl Pts',(22.10992749631,9.16648564567108,-4.42027479233514));
#31013=CARTESIAN_POINT('Ctrl Pts',(22.1631021639207,9.17368437252344,-4.41955354830145));
#31014=CARTESIAN_POINT('Ctrl Pts',(22.2162597933297,9.18041259694753,-4.42001800971797));
#31015=CARTESIAN_POINT('Ctrl Pts',(22.269207906859,9.18664184844023,-4.42169059515386));
#31016=CARTESIAN_POINT('Ctrl Pts',(22.3245959938815,9.1931581584797,-4.42344025725701));
#31017=CARTESIAN_POINT('Ctrl Pts',(22.3798739843465,9.19915414218571,-4.42648583520025));
#31018=CARTESIAN_POINT('Ctrl Pts',(22.4350297409268,9.20463704953186,-4.43079673600685));
#31019=CARTESIAN_POINT('Ctrl Pts',(22.5461903148917,9.21568726741267,-4.43948489908678));
#31020=CARTESIAN_POINT('Ctrl Pts',(22.6568734623399,9.22465589712528,-4.45331387784003));
#31021=CARTESIAN_POINT('Ctrl Pts',(22.7671112483177,9.23161636460099,-4.4720418464562));
#31022=CARTESIAN_POINT('Ctrl Pts',(22.9323771759594,9.24205133573172,-4.50011838190857));
#31023=CARTESIAN_POINT('Ctrl Pts',(23.0966436253579,9.24797370980892,-4.53919106328867));
#31024=CARTESIAN_POINT('Ctrl Pts',(23.2600592455111,9.24956272808001,-4.58811728405156));
#31025=CARTESIAN_POINT('Ctrl Pts',(23.3115335439096,9.25006325306392,-4.60352855798425));
#31026=CARTESIAN_POINT('Ctrl Pts',(23.3626670235205,9.25013116823148,-4.61983815301514));
#31027=CARTESIAN_POINT('Ctrl Pts',(23.4134608761142,9.24978288855012,-4.63697771253073));
#31028=CARTESIAN_POINT('',(30.8496157942439,5.41463414634146,-4.65853571252146));
#31029=CARTESIAN_POINT('Ctrl Pts',(23.4134608743401,9.24978230648852,-4.63697771328011));
#31030=CARTESIAN_POINT('Ctrl Pts',(24.1431288109746,9.24477620324172,-4.63909799546488));
#31031=CARTESIAN_POINT('Ctrl Pts',(24.8609128854776,9.15469739384237,-4.64118229168175));
#31032=CARTESIAN_POINT('Ctrl Pts',(25.9199435996119,8.89326151785136,-4.64425549764083));
#31033=CARTESIAN_POINT('Ctrl Pts',(26.2686099494916,8.78489606818956,-4.64526695104862));
#31034=CARTESIAN_POINT('Ctrl Pts',(26.9440345067492,8.53086155850978,-4.64722569661479));
#31035=CARTESIAN_POINT('Ctrl Pts',(27.2727683495141,8.38474358569576,-4.64817872235552));
#31036=CARTESIAN_POINT('Ctrl Pts',(27.9124127490458,8.05459039487177,-4.65003256384236));
#31037=CARTESIAN_POINT('Ctrl Pts',(28.2233249304724,7.87055863316035,-4.65093338408782));
#31038=CARTESIAN_POINT('Ctrl Pts',(28.8267164809711,7.46328115931847,-4.65268114057206));
#31039=CARTESIAN_POINT('Ctrl Pts',(29.1157096677008,7.24216864268044,-4.65351797766775));
#31040=CARTESIAN_POINT('Ctrl Pts',(29.9348006057639,6.5362496484837,-4.65588924421514));
#31041=CARTESIAN_POINT('Ctrl Pts',(30.4224818233768,6.00624210868884,-4.65730028266099));
#31042=CARTESIAN_POINT('Ctrl Pts',(30.8496157942439,5.41463414634146,-4.65853571252146));
#31043=CARTESIAN_POINT('',(30.8496157942439,5.41463414634146,-3.60555127546399));
#31044=CARTESIAN_POINT('',(30.8496157942439,5.41463414634146,-12.25));
#31045=CARTESIAN_POINT('',(30.4989465761475,5.86984351166101,-2.5869876306867));
#31046=CARTESIAN_POINT('Ctrl Pts',(30.849615794244,5.41463414634146,-3.605551275464));
#31047=CARTESIAN_POINT('Ctrl Pts',(30.7816497053553,5.50877154139453,-3.43196160315339));
#31048=CARTESIAN_POINT('Ctrl Pts',(30.7160583188014,5.59589449756247,-3.25442003177252));
#31049=CARTESIAN_POINT('Ctrl Pts',(30.6537765048508,5.67603715897922,-3.0726189144622));
#31050=CARTESIAN_POINT('Ctrl Pts',(30.5994521176086,5.745940405164,-2.91404558990133));
#31051=CARTESIAN_POINT('Ctrl Pts',(30.547644964311,5.81053321239433,-2.75223195116567));
#31052=CARTESIAN_POINT('Ctrl Pts',(30.4989465761475,5.86984351166102,-2.5869876306867));
#31053=CARTESIAN_POINT('',(29.864460066962,6.56691023510737,-0.418815697553238));
#31054=CARTESIAN_POINT('Ctrl Pts',(30.4989465761475,5.86984351166101,-2.5869876306867));
#31055=CARTESIAN_POINT('Ctrl Pts',(30.4233137302993,5.96195758136262,-2.33034877705622));
#31056=CARTESIAN_POINT('Ctrl Pts',(30.3488530146943,6.04900208546168,-2.07155907215208));
#31057=CARTESIAN_POINT('Ctrl Pts',(30.2763686633504,6.13089490379009,-1.81064777642531));
#31058=CARTESIAN_POINT('Ctrl Pts',(30.2474221995087,6.16359861791162,-1.70645343312763));
#31059=CARTESIAN_POINT('Ctrl Pts',(30.2187907831553,6.19548031299598,-1.60192036444818));
#31060=CARTESIAN_POINT('Ctrl Pts',(30.1905253828516,6.22653294269323,-1.4970490342653));
#31061=CARTESIAN_POINT('Ctrl Pts',(30.1904920035368,6.22656961351661,-1.496925189101));
#31062=CARTESIAN_POINT('Ctrl Pts',(30.1904586247358,6.22660628317995,-1.49680134349088));
#31063=CARTESIAN_POINT('Ctrl Pts',(30.1904252464487,6.22664295168324,-1.49667749743492));
#31064=CARTESIAN_POINT('Ctrl Pts',(30.1409379935327,6.28100833875472,-1.31306109194066));
#31065=CARTESIAN_POINT('Ctrl Pts',(30.0927220038854,6.33270175377753,-1.12832912483359));
#31066=CARTESIAN_POINT('Ctrl Pts',(30.0443718207765,6.38340707955811,-0.943346491560341));
#31067=CARTESIAN_POINT('Ctrl Pts',(30.0441587992402,6.38363047739661,-0.9425314939285));
#31068=CARTESIAN_POINT('Ctrl Pts',(30.043945774759,6.38385385639887,-0.941716493265572));
#31069=CARTESIAN_POINT('Ctrl Pts',(30.043732747184,6.38407721673838,-0.940901489514493));
#31070=CARTESIAN_POINT('Ctrl Pts',(30.0318497332597,6.39653660855655,-0.895439295599127));
#31071=CARTESIAN_POINT('Ctrl Pts',(30.0199872914384,6.40890822298575,-0.849938922706313));
#31072=CARTESIAN_POINT('Ctrl Pts',(30.0079304061828,6.42140928985854,-0.804534650823485));
#31073=CARTESIAN_POINT('Ctrl Pts',(29.9956573763493,6.4341344641823,-0.758316413561679));
#31074=CARTESIAN_POINT('Ctrl Pts',(29.9831839646327,6.44699262206468,-0.712196692305319));
#31075=CARTESIAN_POINT('Ctrl Pts',(29.9702866480314,6.46020934529529,-0.666313906124657));
#31076=CARTESIAN_POINT('Ctrl Pts',(29.9699605773387,6.4605434912446,-0.66515389491177));
#31077=CARTESIAN_POINT('Ctrl Pts',(29.9696342279293,6.46087787433656,-0.663994050439389));
#31078=CARTESIAN_POINT('Ctrl Pts',(29.9693075950715,6.46121249935582,-0.662834372594784));
#31079=CARTESIAN_POINT('Ctrl Pts',(29.9631744517615,6.46749571045688,-0.641059250330851));
#31080=CARTESIAN_POINT('Ctrl Pts',(29.9569646332742,6.47384124142273,-0.619325925282544));
#31081=CARTESIAN_POINT('Ctrl Pts',(29.9504968110584,6.48042900761182,-0.597745652821244));
#31082=CARTESIAN_POINT('Ctrl Pts',(29.9470906715231,6.48389831306226,-0.586380866226969));
#31083=CARTESIAN_POINT('Ctrl Pts',(29.9436136737991,6.48743408574019,-0.575058008090102));
#31084=CARTESIAN_POINT('Ctrl Pts',(29.9400404044472,6.4910615037687,-0.563792529383379));
#31085=CARTESIAN_POINT('Ctrl Pts',(29.9364671350954,6.49468892179722,-0.552527050676656));
#31086=CARTESIAN_POINT('Ctrl Pts',(29.932797593809,6.49840798487454,-0.541318951401599));
#31087=CARTESIAN_POINT('Ctrl Pts',(29.9290063693871,6.50224387307707,-0.530183682526388));
#31088=CARTESIAN_POINT('Ctrl Pts',(29.9286162428098,6.50263859567036,-0.529037835208793));
#31089=CARTESIAN_POINT('Ctrl Pts',(29.9282247857061,6.50303459785586,-0.527892544830234));
#31090=CARTESIAN_POINT('Ctrl Pts',(29.9278319485658,6.50343192910026,-0.526747936182566));
#31091=CARTESIAN_POINT('Ctrl Pts',(29.9263160029589,6.50496521730708,-0.522330929049072));
#31092=CARTESIAN_POINT('Ctrl Pts',(29.9247791427553,6.50651870299062,-0.51791532037233));
#31093=CARTESIAN_POINT('Ctrl Pts',(29.923212672742,6.508100959667,-0.513520375041475));
#31094=CARTESIAN_POINT('Ctrl Pts',(29.9224730227865,6.50884806371013,-0.511445186183043));
#31095=CARTESIAN_POINT('Ctrl Pts',(29.9217268013933,6.50960155180301,-0.509373934703031));
#31096=CARTESIAN_POINT('Ctrl Pts',(29.9209731281652,6.51036229090339,-0.507307791346001));
#31097=CARTESIAN_POINT('Ctrl Pts',(29.9183352718667,6.51302487775473,-0.500076289596397));
#31098=CARTESIAN_POINT('Ctrl Pts',(29.9156061316007,6.51577629047366,-0.492907362352822));
#31099=CARTESIAN_POINT('Ctrl Pts',(29.9127479518585,6.51865369130352,-0.485851205288294));
#31100=CARTESIAN_POINT('Ctrl Pts',(29.9113188619874,6.52009239171845,-0.48232312675603));
#31101=CARTESIAN_POINT('Ctrl Pts',(29.9098575120245,6.52156258893556,-0.478823240768701));
#31102=CARTESIAN_POINT('Ctrl Pts',(29.9083591815029,6.52306892717838,-0.475357821786246));
#31103=CARTESIAN_POINT('Ctrl Pts',(29.9079845988725,6.52344551173908,-0.474491467040632));
#31104=CARTESIAN_POINT('Ctrl Pts',(29.9076077049551,6.52382435511173,-0.473627266482822));
#31105=CARTESIAN_POINT('Ctrl Pts',(29.9072284259906,6.52420552985917,-0.472765318151248));
#31106=CARTESIAN_POINT('Ctrl Pts',(29.9060905890972,6.52534905410146,-0.470179473156526));
#31107=CARTESIAN_POINT('Ctrl Pts',(29.9049312867708,6.52651356070896,-0.467613898198012));
#31108=CARTESIAN_POINT('Ctrl Pts',(29.9037485275245,6.52770100890854,-0.465071240312771));
#31109=CARTESIAN_POINT('Ctrl Pts',(29.9033288342664,6.52812236600652,-0.464168997210231));
#31110=CARTESIAN_POINT('Ctrl Pts',(29.9029063478249,6.52854645079439,-0.463269614505198));
#31111=CARTESIAN_POINT('Ctrl Pts',(29.9024807564583,6.5289735744838,-0.462373498999638));
#31112=CARTESIAN_POINT('Ctrl Pts',(29.9016879290205,6.52976925646165,-0.460704139571641));
#31113=CARTESIAN_POINT('Ctrl Pts',(29.9008844909751,6.53057533159955,-0.459044223607598));
#31114=CARTESIAN_POINT('Ctrl Pts',(29.9000662597657,6.53139594067567,-0.457399865173428));
#31115=CARTESIAN_POINT('Ctrl Pts',(29.8998304861335,6.53163239949107,-0.456926042669205));
#31116=CARTESIAN_POINT('Ctrl Pts',(29.8995935103075,6.53187003887733,-0.45645342429796));
#31117=CARTESIAN_POINT('Ctrl Pts',(29.8993552499751,6.532108940062,-0.455982092705053));
#31118=CARTESIAN_POINT('Ctrl Pts',(29.8992435654444,6.53222092499231,-0.455761156020877));
#31119=CARTESIAN_POINT('Ctrl Pts',(29.8991315986733,6.53233318717316,-0.455540502076082));
#31120=CARTESIAN_POINT('Ctrl Pts',(29.8990193411836,6.53244573497027,-0.455320139382878));
#31121=CARTESIAN_POINT('Ctrl Pts',(29.8989105917404,6.53255476564871,-0.455106663023837));
#31122=CARTESIAN_POINT('Ctrl Pts',(29.8988015694646,6.53266406437131,-0.454893459997586));
#31123=CARTESIAN_POINT('Ctrl Pts',(29.8986922666477,6.53277363874348,-0.454680538042995));
#31124=CARTESIAN_POINT('Ctrl Pts',(29.8969980729862,6.53447204151205,-0.451380247746834));
#31125=CARTESIAN_POINT('Ctrl Pts',(29.8952364806792,6.536236670441,-0.448147484916749));
#31126=CARTESIAN_POINT('Ctrl Pts',(29.8933787760059,6.5380958384941,-0.445011068128653));
#31127=CARTESIAN_POINT('Ctrl Pts',(29.8924499236692,6.53902542252065,-0.443442859734605));
#31128=CARTESIAN_POINT('Ctrl Pts',(29.8914970429738,6.5399786410595,-0.44189873785112));
#31129=CARTESIAN_POINT('Ctrl Pts',(29.8905165433067,6.54095903181656,-0.440382304800807));
#31130=CARTESIAN_POINT('Ctrl Pts',(29.8902714183899,6.54120412950582,-0.440003196538228));
#31131=CARTESIAN_POINT('Ctrl Pts',(29.8900245672838,6.54145092545503,-0.439625818827725));
#31132=CARTESIAN_POINT('Ctrl Pts',(29.8897759338787,6.54169947493436,-0.439250227955585));
#31133=CARTESIAN_POINT('Ctrl Pts',(29.8896826963517,6.54179268098911,-0.439109381378533));
#31134=CARTESIAN_POINT('Ctrl Pts',(29.889589208189,6.54188613363401,-0.438968786075626));
#31135=CARTESIAN_POINT('Ctrl Pts',(29.8894954664315,6.54197983578364,-0.438828445015086));
#31136=CARTESIAN_POINT('Ctrl Pts',(29.8888392741288,6.54263575083105,-0.437846057591307));
#31137=CARTESIAN_POINT('Ctrl Pts',(29.8881706556837,6.54330389161229,-0.436876128043556));
#31138=CARTESIAN_POINT('Ctrl Pts',(29.8874885961489,6.54398525780314,-0.435919674471849));
#31139=CARTESIAN_POINT('Ctrl Pts',(29.8870944326006,6.54437902066664,-0.435366938069227));
#31140=CARTESIAN_POINT('Ctrl Pts',(29.8866948500535,6.54477812955196,-0.434818187012216));
#31141=CARTESIAN_POINT('Ctrl Pts',(29.8862897360135,6.5451826931651,-0.434274045291303));
#31142=CARTESIAN_POINT('Ctrl Pts',(29.8850760327679,6.54639474735693,-0.432643821434411));
#31143=CARTESIAN_POINT('Ctrl Pts',(29.8838119934384,6.54765642037571,-0.431056482531672));
#31144=CARTESIAN_POINT('Ctrl Pts',(29.8824997993162,6.54896534130975,-0.429560752560135));
#31145=CARTESIAN_POINT('Ctrl Pts',(29.8823357196801,6.54912901165925,-0.429373723198144));
#31146=CARTESIAN_POINT('Ctrl Pts',(29.8821708786823,6.5492934291796,-0.429188102306744));
#31147=CARTESIAN_POINT('Ctrl Pts',(29.8820052778696,6.54945859195111,-0.429003977866343));
#31148=CARTESIAN_POINT('Ctrl Pts',(29.8818448520823,6.54961859338601,-0.428825607314705));
#31149=CARTESIAN_POINT('Ctrl Pts',(29.8816837132265,6.54977929422165,-0.428648641147257));
#31150=CARTESIAN_POINT('Ctrl Pts',(29.8815218627084,6.54994069271304,-0.428473159351318));
#31151=CARTESIAN_POINT('Ctrl Pts',(29.8779847464994,6.55346793023428,-0.424638142247988));
#31152=CARTESIAN_POINT('Ctrl Pts',(29.8741093126001,6.55732678218991,-0.421508010922387));
#31153=CARTESIAN_POINT('Ctrl Pts',(29.8699063654193,6.56150301427952,-0.419927508649726));
#31154=CARTESIAN_POINT('Ctrl Pts',(29.8681474715732,6.5632507281113,-0.419266083320906));
#31155=CARTESIAN_POINT('Ctrl Pts',(29.8663314430105,6.56505380581228,-0.418875903796053));
#31156=CARTESIAN_POINT('Ctrl Pts',(29.864460066962,6.56691023510737,-0.418815697553239));
#31157=CARTESIAN_POINT('Ctrl Pts',(29.864460066962,6.56691023510738,-0.418815697553238));
#31158=CARTESIAN_POINT('Ctrl Pts',(29.4803688233762,6.9479337269518,-0.406458645803864));
#31159=CARTESIAN_POINT('Ctrl Pts',(29.0688833692417,7.28992300517486,-0.3927064137635));
#31160=CARTESIAN_POINT('Ctrl Pts',(28.6310287709774,7.59430983868232,-0.377052593566359));
#31161=CARTESIAN_POINT('Ctrl Pts',(28.5761396683459,7.63246752895278,-0.375090243172456));
#31162=CARTESIAN_POINT('Ctrl Pts',(28.5208361379456,7.67003424468116,-0.373098007376688));
#31163=CARTESIAN_POINT('Ctrl Pts',(28.4651201665043,7.70701275996229,-0.371074886541032));
#31164=CARTESIAN_POINT('Ctrl Pts',(28.4648104733999,7.70721830230314,-0.371063641173575));
#31165=CARTESIAN_POINT('Ctrl Pts',(28.4645007674488,7.70742382634658,-0.371052394838906));
#31166=CARTESIAN_POINT('Ctrl Pts',(28.4641910486506,7.70762933209214,-0.371041147536674));
#31167=CARTESIAN_POINT('Ctrl Pts',(28.214388439779,7.87337926936937,-0.361969675425142));
#31168=CARTESIAN_POINT('Ctrl Pts',(27.9562330077088,8.02722271600796,-0.35226895739612));
#31169=CARTESIAN_POINT('Ctrl Pts',(27.6895545622681,8.16889014500123,-0.341754746575349));
#31170=CARTESIAN_POINT('Ctrl Pts',(27.6890674556282,8.16914891036643,-0.341735541641497));
#31171=CARTESIAN_POINT('Ctrl Pts',(27.6885803173177,8.16940763590204,-0.341716333849271));
#31172=CARTESIAN_POINT('Ctrl Pts',(27.6880931473781,8.16966632158906,-0.341697123198757));
#31173=CARTESIAN_POINT('Ctrl Pts',(27.4215277388687,8.31121170489137,-0.331185606609609));
#31174=CARTESIAN_POINT('Ctrl Pts',(27.1454796620243,8.44083288074727,-0.319817779335625));
#31175=CARTESIAN_POINT('Ctrl Pts',(26.8667371201343,8.55541115481146,-0.307607446891298));
#31176=CARTESIAN_POINT('Ctrl Pts',(26.8660732568102,8.55568403857499,-0.307578366321717));
#31177=CARTESIAN_POINT('Ctrl Pts',(26.8654093710373,8.55595684207196,-0.30754928159864));
#31178=CARTESIAN_POINT('Ctrl Pts',(26.8647454628164,8.55622956530339,-0.307520192712224));
#31179=CARTESIAN_POINT('Ctrl Pts',(26.3393506191311,8.77205364316396,-0.284500217281987));
#31180=CARTESIAN_POINT('Ctrl Pts',(25.799870653803,8.93761716527978,-0.25887481178718));
#31181=CARTESIAN_POINT('Ctrl Pts',(25.2467440839775,9.05344973047515,-0.225765235501146));
#31182=CARTESIAN_POINT('Ctrl Pts',(25.2124847851188,9.06062411457651,-0.223714509806617));
#31183=CARTESIAN_POINT('Ctrl Pts',(25.1781731384515,9.06760773287862,-0.221635078942255));
#31184=CARTESIAN_POINT('Ctrl Pts',(25.143809249779,9.0744007171519,-0.219525786381147));
#31185=CARTESIAN_POINT('Ctrl Pts',(25.1428439684928,9.07459153201161,-0.219466536374384));
#31186=CARTESIAN_POINT('Ctrl Pts',(25.1418786392007,9.07478219599054,-0.21940726454339));
#31187=CARTESIAN_POINT('Ctrl Pts',(25.1409132619708,9.07497270906429,-0.219347970745587));
#31188=CARTESIAN_POINT('Ctrl Pts',(24.8468326636315,9.13300825930098,-0.201285440372893));
#31189=CARTESIAN_POINT('Ctrl Pts',(24.5482782341044,9.17704104931834,-0.181185608761272));
#31190=CARTESIAN_POINT('Ctrl Pts',(24.2472922152141,9.20637641423141,-0.155024952944712));
#31191=CARTESIAN_POINT('Ctrl Pts',(24.2462473257163,9.20647825356211,-0.154934134791034));
#31192=CARTESIAN_POINT('Ctrl Pts',(24.2452024316097,9.20657991366609,-0.154843252774193));
#31193=CARTESIAN_POINT('Ctrl Pts',(24.2441575329877,9.20668139455152,-0.154752305929168));
#31194=CARTESIAN_POINT('Ctrl Pts',(24.0941447324839,9.22125068529444,-0.14169535415231));
#31195=CARTESIAN_POINT('Ctrl Pts',(23.9440399212374,9.23212605584461,-0.127301668598929));
#31196=CARTESIAN_POINT('Ctrl Pts',(23.7940966118025,9.2393332118484,-0.108714691115995));
#31197=CARTESIAN_POINT('Ctrl Pts',(23.7930931044887,9.23938144630307,-0.108590296316943));
#31198=CARTESIAN_POINT('Ctrl Pts',(23.7920895941272,9.23942951656461,-0.108465732409656));
#31199=CARTESIAN_POINT('Ctrl Pts',(23.7910860815245,9.23947742263663,-0.108340994413874));
#31200=CARTESIAN_POINT('Ctrl Pts',(23.7165180424478,9.24303718047232,-0.0990720846670683));
#31201=CARTESIAN_POINT('Ctrl Pts',(23.6420034506113,9.24568741560599,-0.0888545330623582));
#31202=CARTESIAN_POINT('Ctrl Pts',(23.5678498899834,9.24743431582237,-0.0756482682786467));
#31203=CARTESIAN_POINT('Ctrl Pts',(23.5669491575255,9.24745553516386,-0.0754878537113851));
#31204=CARTESIAN_POINT('Ctrl Pts',(23.5660485062894,9.24747662022085,-0.0753270522346912));
#31205=CARTESIAN_POINT('Ctrl Pts',(23.5651479404179,9.24749757107011,-0.0751658425171525));
#31206=CARTESIAN_POINT('Ctrl Pts',(23.5284025808081,9.24835241857714,-0.0685880793227154));
#31207=CARTESIAN_POINT('Ctrl Pts',(23.4918351889453,9.2489830059991,-0.0613344717879373));
#31208=CARTESIAN_POINT('Ctrl Pts',(23.4557284619252,9.24939573660609,-0.0519736470563747));
#31209=CARTESIAN_POINT('Ctrl Pts',(23.4549670822659,9.24940443982333,-0.0517762560953804));
#31210=CARTESIAN_POINT('Ctrl Pts',(23.4542058832591,9.24941304616209,-0.0515780514109144));
#31211=CARTESIAN_POINT('Ctrl Pts',(23.4534448814482,9.24942155576376,-0.0513789487714902));
#31212=CARTESIAN_POINT('Ctrl Pts',(23.4356451193329,9.24962059456144,-0.0467219564126235));
#31213=CARTESIAN_POINT('Ctrl Pts',(23.4179889581537,9.24976631161214,-0.0415791200096051));
#31214=CARTESIAN_POINT('Ctrl Pts',(23.4006884106516,9.24986111707689,-0.034896743815993));
#31215=CARTESIAN_POINT('Ctrl Pts',(23.4000808005074,9.24986444672655,-0.0346620530027444));
#31216=CARTESIAN_POINT('Ctrl Pts',(23.3994734618759,9.24986771271723,-0.0344255895231507));
#31217=CARTESIAN_POINT('Ctrl Pts',(23.3988665594379,9.24987091524699,-0.0341871261202171));
#31218=CARTESIAN_POINT('Ctrl Pts',(23.393194545426,9.24990084558269,-0.0319584849449891));
#31219=CARTESIAN_POINT('Ctrl Pts',(23.3875779991193,9.24992512955467,-0.0295571279873106));
#31220=CARTESIAN_POINT('Ctrl Pts',(23.3821729808622,9.24994398093205,-0.026804837660644));
#31221=CARTESIAN_POINT('Ctrl Pts',(23.3794776955015,9.24995338142601,-0.0254323709134002));
#31222=CARTESIAN_POINT('Ctrl Pts',(23.3768348453943,9.24996143411909,-0.0239732602558811));
#31223=CARTESIAN_POINT('Ctrl Pts',(23.3742624517826,9.2499681827706,-0.0224103397596845));
#31224=CARTESIAN_POINT('Ctrl Pts',(23.3738593623926,9.24996924027199,-0.0221654329668209));
#31225=CARTESIAN_POINT('Ctrl Pts',(23.3734522044323,9.24997026479149,-0.021918200656897));
#31226=CARTESIAN_POINT('Ctrl Pts',(23.3730424270331,9.24997125713655,-0.0216682085089925));
#31227=CARTESIAN_POINT('Ctrl Pts',(23.369904732602,9.24997885559263,-0.0197540010101278));
#31228=CARTESIAN_POINT('Ctrl Pts',(23.3666181492267,9.24998457304712,-0.017712833015035));
#31229=CARTESIAN_POINT('Ctrl Pts',(23.3637877463315,9.24998876199755,-0.0153303479388135));
#31230=CARTESIAN_POINT('Ctrl Pts',(23.3598235387692,9.24999462896053,-0.0119934854121405));
#31231=CARTESIAN_POINT('Ctrl Pts',(23.3567454098863,9.24999749331721,-0.00798953227686465));
#31232=CARTESIAN_POINT('Ctrl Pts',(23.3561574375587,9.24999819731105,-0.00274506802632453));
#31233=CARTESIAN_POINT('Ctrl Pts',(23.3560588672729,9.24999831533169,-0.00186586280564814));
#31234=CARTESIAN_POINT('Ctrl Pts',(23.3560304040022,9.24999837253056,-0.000951760491110045));
#31235=CARTESIAN_POINT('Ctrl Pts',(23.3560798277435,9.24999837277875,-1.98299169792971E-9));
#31236=CARTESIAN_POINT('Origin',(31.6603850692973,-6.,-12.25));
#31237=CARTESIAN_POINT('',(31.6603850692973,-5.,-3.60555127546388));
#31238=CARTESIAN_POINT('Origin',(31.6603850692973,-6.,-3.60555127546399));
#31239=CARTESIAN_POINT('',(31.6603850692973,-5.,-4.65853571252147));
#31240=CARTESIAN_POINT('',(31.6603850692973,-5.,-12.25));
#31241=CARTESIAN_POINT('Origin',(31.6603850692973,-6.,-4.65853571252147));
#31242=CARTESIAN_POINT('Origin',(31.6603850692973,6.,-12.25));
#31243=CARTESIAN_POINT('',(31.6603850692973,5.,-4.65853571252146));
#31244=CARTESIAN_POINT('Origin',(31.6603850692973,6.,-4.65853571252146));
#31245=CARTESIAN_POINT('',(31.6603850692973,5.,-3.60555127546399));
#31246=CARTESIAN_POINT('',(31.6603850692973,5.,-12.25));
#31247=CARTESIAN_POINT('Origin',(31.6603850692973,6.,-3.60555127546399));
#31248=CARTESIAN_POINT('Origin',(31.6603850692973,5.,-12.25));
#31249=CARTESIAN_POINT('',(32.1691171325868,5.,-3.60555127546399));
#31250=CARTESIAN_POINT('Origin',(23.3621596556826,5.,0.));
#31251=CARTESIAN_POINT('',(31.6603850692973,5.,-3.60555127546399));
#31252=CARTESIAN_POINT('Origin',(31.6603850692973,-5.,-12.25));
#31253=CARTESIAN_POINT('',(31.6603850692973,-5.,-3.60555127546388));
#31254=CARTESIAN_POINT('Origin',(23.3621596556826,-5.00000000000001,0.));
#31255=CARTESIAN_POINT('Ctrl Pts',(29.9256651987116,6.61722146123576,-0.0297557807112802));
#31256=CARTESIAN_POINT('Ctrl Pts',(29.8674234378362,6.56397053279327,-0.216304525438927));
#31257=CARTESIAN_POINT('Ctrl Pts',(29.864460066962,6.56691023510738,-0.418815697553239));
#31258=CARTESIAN_POINT('Ctrl Pts',(29.4859454402383,7.0470527099288,-0.0278002419024762));
#31259=CARTESIAN_POINT('Ctrl Pts',(29.4356629944171,6.99266939386707,-0.209154663943272));
#31260=CARTESIAN_POINT('Ctrl Pts',(29.432253356123,6.99566489409161,-0.404910666487137));
#31261=CARTESIAN_POINT('Ctrl Pts',(29.0122518974518,7.42509242577045,-0.0257317744209179));
#31262=CARTESIAN_POINT('Ctrl Pts',(28.9691053861043,7.37213789927329,-0.20109030922603));
#31263=CARTESIAN_POINT('Ctrl Pts',(28.9652970371725,7.37504694162835,-0.389236972852743));
#31264=CARTESIAN_POINT('Ctrl Pts',(28.2541034544046,7.91872357544883,-0.0225015885182954));
#31265=CARTESIAN_POINT('Ctrl Pts',(28.2193066048444,7.87034913000682,-0.187059634742587));
#31266=CARTESIAN_POINT('Ctrl Pts',(28.2150317307479,7.87299566940952,-0.36199386194761));
#31267=CARTESIAN_POINT('Ctrl Pts',(27.9927306925325,8.07123684933647,-0.0214007247497678));
#31268=CARTESIAN_POINT('Ctrl Pts',(27.9610163781938,8.02448959484978,-0.182056771104165));
#31269=CARTESIAN_POINT('Ctrl Pts',(27.9565703991337,8.02704348376819,-0.35228226385434));
#31270=CARTESIAN_POINT('Ctrl Pts',(27.4532829707667,8.35132766261088,-0.0191573375898124));
#31271=CARTESIAN_POINT('Ctrl Pts',(27.4273020987592,8.30839838388361,-0.171205631262116));
#31272=CARTESIAN_POINT('Ctrl Pts',(27.4225387252865,8.31073680629592,-0.331227233479106));
#31273=CARTESIAN_POINT('Ctrl Pts',(27.1741459407437,8.4790792417291,-0.0180108315948677));
#31274=CARTESIAN_POINT('Ctrl Pts',(27.1509110455396,8.43840855393471,-0.165335158707994));
#31275=CARTESIAN_POINT('Ctrl Pts',(27.1459961653766,8.44062057060429,-0.319840425193462));
#31276=CARTESIAN_POINT('Ctrl Pts',(26.3281384957242,8.8170194343566,-0.0145767734067967));
#31277=CARTESIAN_POINT('Ctrl Pts',(26.3136110967992,8.78315925951623,-0.146408797766953));
#31278=CARTESIAN_POINT('Ctrl Pts',(26.3082189750152,8.78499234568301,-0.283143105918742));
#31279=CARTESIAN_POINT('Ctrl Pts',(25.7498122714157,8.98393143595614,-0.012298136026498));
#31280=CARTESIAN_POINT('Ctrl Pts',(25.7393784856676,8.95628810851345,-0.13226590849984));
#31281=CARTESIAN_POINT('Ctrl Pts',(25.7337629487011,8.95777986606531,-0.255738121840876));
#31282=CARTESIAN_POINT('Ctrl Pts',(24.8625853761885,9.14937514280772,-0.00875627031697524));
#31283=CARTESIAN_POINT('Ctrl Pts',(24.854581000935,9.13176556219335,-0.104200610475345));
#31284=CARTESIAN_POINT('Ctrl Pts',(24.8488322355087,9.13271117527109,-0.201422710339758));
#31285=CARTESIAN_POINT('Ctrl Pts',(24.5621172854782,9.19032444121584,-0.00755656773431116));
#31286=CARTESIAN_POINT('Ctrl Pts',(24.5551525359009,9.17617850406612,-0.0937897668906999));
#31287=CARTESIAN_POINT('Ctrl Pts',(24.5493473176572,9.17693685209554,-0.18127855553775));
#31288=CARTESIAN_POINT('Ctrl Pts',(24.108465748896,9.22946475773662,-0.00557635783698352));
#31289=CARTESIAN_POINT('Ctrl Pts',(24.102103013715,9.2206234248347,-0.0734246424062645));
#31290=CARTESIAN_POINT('Ctrl Pts',(24.0962646566383,9.22109619601611,-0.14189824629866));
#31291=CARTESIAN_POINT('Ctrl Pts',(23.9570760406083,9.23875711818494,-0.00489255841352439));
#31292=CARTESIAN_POINT('Ctrl Pts',(23.9509623379496,9.2316974291279,-0.0659443870662256));
#31293=CARTESIAN_POINT('Ctrl Pts',(23.9451103869989,9.23207461096955,-0.127435185338512));
#31294=CARTESIAN_POINT('Ctrl Pts',(23.7304221300224,9.24710877356689,-0.00369560630858036));
#31295=CARTESIAN_POINT('Ctrl Pts',(23.7244488524214,9.24272883655924,-0.0514200221845465));
#31296=CARTESIAN_POINT('Ctrl Pts',(23.7185889926675,9.24296254743522,-0.099360999755311));
#31297=CARTESIAN_POINT('Ctrl Pts',(23.6548365752529,9.24896093156313,-0.0032714230986638));
#31298=CARTESIAN_POINT('Ctrl Pts',(23.6489217801125,9.24547672099602,-0.0460828268538334));
#31299=CARTESIAN_POINT('Ctrl Pts',(23.6430586656839,9.24566255860898,-0.0890452900807008));
#31300=CARTESIAN_POINT('Ctrl Pts',(23.5419950086281,9.25035039840065,-0.00249198665734557));
#31301=CARTESIAN_POINT('Ctrl Pts',(23.5361101102027,9.24820589361364,-0.0356850645088389));
#31302=CARTESIAN_POINT('Ctrl Pts',(23.5302452018341,9.24832020150227,-0.068951626680926));
#31303=CARTESIAN_POINT('Ctrl Pts',(23.5045077861791,9.25058086470768,-0.00221154209606147));
#31304=CARTESIAN_POINT('Ctrl Pts',(23.4986354745838,9.24888177359471,-0.0318691204795911));
#31305=CARTESIAN_POINT('Ctrl Pts',(23.4927698292697,9.2489723231015,-0.0615775234007954));
#31306=CARTESIAN_POINT('Ctrl Pts',(23.4489407653687,9.25059023689579,-0.00168033373592259));
#31307=CARTESIAN_POINT('Ctrl Pts',(23.4430734758481,9.24955214356626,-0.0244145411752795));
#31308=CARTESIAN_POINT('Ctrl Pts',(23.4372074649957,9.24960744693854,-0.0471730480279435));
#31309=CARTESIAN_POINT('Ctrl Pts',(23.430512099699,9.2505372510034,-0.00148734722344965));
#31310=CARTESIAN_POINT('Ctrl Pts',(23.4246470785189,9.24971834747212,-0.0216787626321344));
#31311=CARTESIAN_POINT('Ctrl Pts',(23.4187809144113,9.24976197463182,-0.0418867767978843));
#31312=CARTESIAN_POINT('Ctrl Pts',(23.403371063412,9.25038009688579,-0.00111076356707283));
#31313=CARTESIAN_POINT('Ctrl Pts',(23.3975061807919,9.24988429559992,-0.0162555467205808));
#31314=CARTESIAN_POINT('Ctrl Pts',(23.3916399614818,9.24991070032524,-0.0314080342307533));
#31315=CARTESIAN_POINT('Ctrl Pts',(23.3943702298556,9.25031441825653,-0.000971660015808843));
#31316=CARTESIAN_POINT('Ctrl Pts',(23.3885054832099,9.24992551808104,-0.0142418469089325));
#31317=CARTESIAN_POINT('Ctrl Pts',(23.3826392408467,9.24994623900693,-0.0275171890143565));
#31318=CARTESIAN_POINT('Ctrl Pts',(23.3775485047153,9.25016841960209,-0.000613695653578594));
#31319=CARTESIAN_POINT('Ctrl Pts',(23.3716836057147,9.24998029042593,-0.00902103423512527));
#31320=CARTESIAN_POINT('Ctrl Pts',(23.3658173417984,9.24999030033329,-0.0174297620702533));
#31321=CARTESIAN_POINT('Ctrl Pts',(23.3672236677921,9.24999842822739,-0.000399711082514158));
#31322=CARTESIAN_POINT('Ctrl Pts',(23.3613578848224,9.24999839902789,-0.0058628102385145));
#31323=CARTESIAN_POINT('Ctrl Pts',(23.3554916518206,9.24999836982608,-0.0113265471363916));
#31324=CARTESIAN_POINT('Ctrl Pts',(23.3560798278466,9.24999837277863,1.1114590155748E-11));
#31325=CARTESIAN_POINT('Ctrl Pts',(23.3560798278471,9.24999837277875,1.11145901557479E-11));
#31326=CARTESIAN_POINT('Ctrl Pts',(23.3560798278471,9.24999837277875,1.11145901557479E-11));
#31327=CARTESIAN_POINT('Origin',(30.568726020147,7.2768464767406,-0.41881569755326));
#31328=CARTESIAN_POINT('Ctrl Pts',(29.8644600065632,6.56691029503575,-0.418819825507771));
#31329=CARTESIAN_POINT('Ctrl Pts',(29.8647590574648,6.56661351376205,-0.398379188670332));
#31330=CARTESIAN_POINT('Ctrl Pts',(29.8656463748335,6.56691023510728,-0.377955629499233));
#31331=CARTESIAN_POINT('Ctrl Pts',(29.8728343714978,6.55860281663837,-0.419091850166062));
#31332=CARTESIAN_POINT('Ctrl Pts',(29.8782115436644,6.55326768870704,-0.398348099807103));
#31333=CARTESIAN_POINT('Ctrl Pts',(29.884200490205,6.54855448701688,-0.377622540410929));
#31334=CARTESIAN_POINT('Ctrl Pts',(29.8800819130269,6.55138207515269,-0.425969995675749));
#31335=CARTESIAN_POINT('Ctrl Pts',(29.8897499363818,6.54175217037167,-0.404642020874189));
#31336=CARTESIAN_POINT('Ctrl Pts',(29.9002720486976,6.53300459397134,-0.38333825478346));
#31337=CARTESIAN_POINT('Ctrl Pts',(29.8924907668869,6.53899009410551,-0.442589318556842));
#31338=CARTESIAN_POINT('Ctrl Pts',(29.9094054806592,6.52207290338313,-0.419992353306782));
#31339=CARTESIAN_POINT('Ctrl Pts',(29.9277760758933,6.50668389169176,-0.397441088483466));
#31340=CARTESIAN_POINT('Ctrl Pts',(29.8976669478591,6.53380470607085,-0.45228876882253));
#31341=CARTESIAN_POINT('Ctrl Pts',(29.9175524482434,6.51388066947101,-0.429013649275077));
#31342=CARTESIAN_POINT('Ctrl Pts',(29.9392488830213,6.49587018835024,-0.405796768245691));
#31343=CARTESIAN_POINT('Ctrl Pts',(29.9120903594397,6.51932939050281,-0.482562048497315));
#31344=CARTESIAN_POINT('Ctrl Pts',(29.9401818870522,6.49106922804923,-0.457204813104785));
#31345=CARTESIAN_POINT('Ctrl Pts',(29.9712179947108,6.46598442274517,-0.431945103081834));
#31346=CARTESIAN_POINT('Ctrl Pts',(29.9202056092526,6.51114549543016,-0.504588759159602));
#31347=CARTESIAN_POINT('Ctrl Pts',(29.9527979603682,6.47826656633695,-0.477763194146236));
#31348=CARTESIAN_POINT('Ctrl Pts',(29.9892051112283,6.44954244731878,-0.451072033579264));
#31349=CARTESIAN_POINT('Ctrl Pts',(29.9430602275497,6.48802947551604,-0.571085079784156));
#31350=CARTESIAN_POINT('Ctrl Pts',(29.9881729418631,6.44222489898683,-0.539807241634622));
#31351=CARTESIAN_POINT('Ctrl Pts',(30.0398614866482,6.40380994709606,-0.508771304298676));
#31352=CARTESIAN_POINT('Ctrl Pts',(29.956339107267,6.47449825530805,-0.616854862246528));
#31353=CARTESIAN_POINT('Ctrl Pts',(30.0084689143173,6.4213325472565,-0.582474942809098));
#31354=CARTESIAN_POINT('Ctrl Pts',(30.0692934500721,6.3780928359179,-0.548455864922925));
#31355=CARTESIAN_POINT('Ctrl Pts',(29.995208562426,6.4346778775047,-0.754816375285201));
#31356=CARTESIAN_POINT('Ctrl Pts',(30.0675109303063,6.36011843264923,-0.710896214022496));
#31357=CARTESIAN_POINT('Ctrl Pts',(30.1554454871045,6.30433955874164,-0.66767816099171));
#31358=CARTESIAN_POINT('Ctrl Pts',(30.0194181045814,6.40957107285731,-0.847960985155597));
#31359=CARTESIAN_POINT('Ctrl Pts',(30.1036626071983,6.32199819104647,-0.797244914477581));
#31360=CARTESIAN_POINT('Ctrl Pts',(30.2091042861041,6.26062352799595,-0.747681437960539));
#31361=CARTESIAN_POINT('Ctrl Pts',(30.092304518959,6.33314980954348,-1.12681711647389));
#31362=CARTESIAN_POINT('Ctrl Pts',(30.2115890006386,6.20653143108887,-1.0550333875945));
#31363=CARTESIAN_POINT('Ctrl Pts',(30.3706514596258,6.13374391009409,-0.985820942249229));
#31364=CARTESIAN_POINT('Ctrl Pts',(30.1407348577505,6.28123094419676,-1.31242838622513));
#31365=CARTESIAN_POINT('Ctrl Pts',(30.2817692847275,6.12909735050055,-1.22513859180251));
#31366=CARTESIAN_POINT('Ctrl Pts',(30.4779926802797,6.05598466186384,-1.1425333971258));
#31367=CARTESIAN_POINT('Ctrl Pts',(30.2897107926523,6.11757159098365,-1.86523612312724));
#31368=CARTESIAN_POINT('Ctrl Pts',(30.4962880035196,5.88480475057273,-1.72974568641597));
#31369=CARTESIAN_POINT('Ctrl Pts',(30.8081817131166,5.83224880525388,-1.60732611923157));
#31370=CARTESIAN_POINT('Ctrl Pts',(30.3933751772269,5.99841777185359,-2.22895100183562));
#31371=CARTESIAN_POINT('Ctrl Pts',(30.6429929060619,5.70670516719143,-2.05647096278954));
#31372=CARTESIAN_POINT('Ctrl Pts',(31.037876828135,5.69732008134285,-1.910419085916));
#31373=CARTESIAN_POINT('Ctrl Pts',(30.4988949496231,5.86990639476642,-2.58702950046792));
#31374=CARTESIAN_POINT('Ctrl Pts',(30.7855691211664,5.52068951837422,-2.35451845566136));
#31375=CARTESIAN_POINT('Ctrl Pts',(31.2718056654608,5.57521816165486,-2.21741796916003));
#31376=CARTESIAN_POINT('Origin',(31.2718056654608,6.50442118859734,-2.5869876306867));
#31377=CARTESIAN_POINT('Ctrl Pts',(30.4952922544597,5.87429133954168,-2.57456137435286));
#31378=CARTESIAN_POINT('Ctrl Pts',(30.782100878076,5.52542682926995,-2.34331966444516));
#31379=CARTESIAN_POINT('Ctrl Pts',(31.2677682718457,5.57944414885034,-2.20676332755905));
#31380=CARTESIAN_POINT('Ctrl Pts',(30.6026936291125,5.74365115677448,-2.94054961542787));
#31381=CARTESIAN_POINT('Ctrl Pts',(30.8866588414079,5.38513818004545,-2.67536548263577));
#31382=CARTESIAN_POINT('Ctrl Pts',(31.3867827859923,5.45535959932825,-2.5204722442975));
#31383=CARTESIAN_POINT('Ctrl Pts',(30.7245581660918,5.58814855489033,-3.28694957844283));
#31384=CARTESIAN_POINT('Ctrl Pts',(31.0038498616718,5.21939244642611,-2.98485241905066));
#31385=CARTESIAN_POINT('Ctrl Pts',(31.5218261370795,5.30765757528954,-2.81739272720526));
#31386=CARTESIAN_POINT('Ctrl Pts',(30.8540107833037,5.40854159977948,-3.61676245692539));
#31387=CARTESIAN_POINT('Ctrl Pts',(31.12465101472,5.03304526371785,-3.27244402072503));
#31388=CARTESIAN_POINT('Ctrl Pts',(31.6652680269827,5.1370731461929,-3.10007755423114));
#31389=CARTESIAN_POINT('Origin',(31.6603850692973,6.,-3.60555127546399));
#31390=CARTESIAN_POINT('Origin',(31.6603850692973,6.,-3.60555127546399));
#31391=CARTESIAN_POINT('Origin',(31.6603850692973,6.,-3.60555127546399));
#31392=CARTESIAN_POINT('Origin',(-60.4312629272455,6.,-3.60555127546399));
#31393=CARTESIAN_POINT('Origin',(32.1691171325868,6.,-3.60555127546399));
#31394=CARTESIAN_POINT('Origin',(32.1691171325868,6.,-3.60555127546399));
#31395=CARTESIAN_POINT('Origin',(32.1691171325868,6.,-3.60555127546399));
#31396=CARTESIAN_POINT('Origin',(23.3621596556826,6.,0.));
#31397=CARTESIAN_POINT('Origin',(31.6603850692973,6.,-4.65853571252146));
#31398=CARTESIAN_POINT('Origin',(31.6603850692973,6.,-4.65853571252146));
#31399=CARTESIAN_POINT('Origin',(31.6603850692973,6.,-4.65853571252146));
#31400=CARTESIAN_POINT('Ctrl Pts',(30.8533045357049,5.40952138492279,-4.65854638171787));
#31401=CARTESIAN_POINT('Ctrl Pts',(30.8491863429757,5.41523354504457,-9.27174184878108));
#31402=CARTESIAN_POINT('Ctrl Pts',(32.4024604985946,6.5271674864424,-5.07262713991702));
#31403=CARTESIAN_POINT('Ctrl Pts',(30.4152070763528,6.01717418209453,-4.65727924423286));
#31404=CARTESIAN_POINT('Ctrl Pts',(30.4100357196704,6.02337177530084,-9.27185079335277));
#31405=CARTESIAN_POINT('Ctrl Pts',(31.8738489475746,7.26036572944057,-5.07124736770548));
#31406=CARTESIAN_POINT('Ctrl Pts',(29.9132343908611,6.56007337163006,-4.65582684825921));
#31407=CARTESIAN_POINT('Ctrl Pts',(29.9069965319543,6.56635458454684,-9.27197690984398));
#31408=CARTESIAN_POINT('Ctrl Pts',(31.2681650881604,7.91543180449786,-5.06966586821974));
#31409=CARTESIAN_POINT('Ctrl Pts',(29.0687996562968,7.27970396316172,-4.65338215219011));
#31410=CARTESIAN_POINT('Ctrl Pts',(29.0612810766789,7.28562977259251,-9.27219266300731));
#31411=CARTESIAN_POINT('Ctrl Pts',(30.249264051552,8.78374326273839,-5.06700386436201));
#31412=CARTESIAN_POINT('Ctrl Pts',(28.7706261881112,7.5045195286773,-4.6525187043648));
#31413=CARTESIAN_POINT('Ctrl Pts',(28.7626222317122,7.51031058117165,-9.27226941720389));
#31414=CARTESIAN_POINT('Ctrl Pts',(29.8894857961232,9.05500734423689,-5.06606366510161));
#31415=CARTESIAN_POINT('Ctrl Pts',(28.1502182742168,7.91573787763403,-4.65072158676973));
#31416=CARTESIAN_POINT('Ctrl Pts',(28.1413123183606,7.92115484475472,-9.27243052035246));
#31417=CARTESIAN_POINT('Ctrl Pts',(29.1408971363909,9.55118636769414,-5.06410680227826));
#31418=CARTESIAN_POINT('Ctrl Pts',(27.8303931769536,8.10087907780226,-4.64979489842099));
#31419=CARTESIAN_POINT('Ctrl Pts',(27.821054471481,8.10605040905191,-9.272514243178));
#31420=CARTESIAN_POINT('Ctrl Pts',(28.7549938692442,9.77457907404743,-5.06309774114946));
#31421=CARTESIAN_POINT('Ctrl Pts',(27.1720888828603,8.43147682347415,-4.64788686746487));
#31422=CARTESIAN_POINT('Ctrl Pts',(27.1619692903368,8.43607716328527,-9.27268812714177));
#31423=CARTESIAN_POINT('Ctrl Pts',(27.9606791639968,10.1734806965365,-5.06102010612049));
#31424=CARTESIAN_POINT('Ctrl Pts',(26.8336084090208,8.57693065213341,-4.64690552139546));
#31425=CARTESIAN_POINT('Ctrl Pts',(26.8231243399102,8.58119242091901,-9.27277829295943));
#31426=CARTESIAN_POINT('Ctrl Pts',(27.5522661850684,10.3489863345083,-5.05995152857685));
#31427=CARTESIAN_POINT('Ctrl Pts',(26.1377630016309,8.82766358702257,-4.6448874029651));
#31428=CARTESIAN_POINT('Ctrl Pts',(26.126651484303,8.83118310305817,-9.27296539649604));
#31429=CARTESIAN_POINT('Ctrl Pts',(26.7126541019231,10.6515225006985,-5.05775402063852));
#31430=CARTESIAN_POINT('Ctrl Pts',(25.7778982955421,8.93339034065304,-4.64384337398826));
#31431=CARTESIAN_POINT('Ctrl Pts',(25.7665078239556,8.93648699505822,-9.27306302842017));
#31432=CARTESIAN_POINT('Ctrl Pts',(26.2784387542334,10.7790931636271,-5.05661718840979));
#31433=CARTESIAN_POINT('Ctrl Pts',(24.6929742515822,9.18202225043397,-4.64069473154187));
#31434=CARTESIAN_POINT('Ctrl Pts',(24.6806743997377,9.18386771107264,-9.27336026701771));
#31435=CARTESIAN_POINT('Ctrl Pts',(24.9693615852528,11.0790942178401,-5.05318866422855));
#31436=CARTESIAN_POINT('Ctrl Pts',(23.9606020319037,9.25954965162327,-4.63856783364716));
#31437=CARTESIAN_POINT('Ctrl Pts',(23.9480649578887,9.26034679384474,-9.27356456880832));
#31438=CARTESIAN_POINT('Ctrl Pts',(24.0856759871578,11.1726393389832,-5.05087270788839));
#31439=CARTESIAN_POINT('Ctrl Pts',(23.2193295343223,9.24907699337613,-4.63641356863091));
#31440=CARTESIAN_POINT('Ctrl Pts',(23.207169819274,9.2489052015715,-9.27377520050726));
#31441=CARTESIAN_POINT('Ctrl Pts',(23.1912512483198,11.1600029543463,-5.04852695082781));
#31442=CARTESIAN_POINT('Ctrl Pts',(23.3608199269989,11.1532729634477,-5.06590970436805));
#31443=CARTESIAN_POINT('Ctrl Pts',(23.3559710985418,11.138801958104,-5.09636870971951));
#31444=CARTESIAN_POINT('Ctrl Pts',(23.3512201232246,11.1227796717029,-5.12610035313048));
#31445=CARTESIAN_POINT('Ctrl Pts',(23.3465896271706,11.1053240247021,-5.15490162040772));
#31446=CARTESIAN_POINT('Ctrl Pts',(23.3418797587551,11.0875691665787,-5.18419657660481));
#31447=CARTESIAN_POINT('Ctrl Pts',(23.3372945494785,11.0683328667465,-5.21252880312016));
#31448=CARTESIAN_POINT('Ctrl Pts',(23.3328562035503,11.0477509482033,-5.23973798876087));
#31449=CARTESIAN_POINT('Ctrl Pts',(23.3283351879441,11.0267856659916,-5.26745397910974));
#31450=CARTESIAN_POINT('Ctrl Pts',(23.3239665585533,11.0044256733813,-5.29400517632869));
#31451=CARTESIAN_POINT('Ctrl Pts',(23.3197720151725,10.980803455366,-5.31927492433835));
#31452=CARTESIAN_POINT('Ctrl Pts',(23.3154580131966,10.9565084878478,-5.34526434271944));
#31453=CARTESIAN_POINT('Ctrl Pts',(23.3113281462826,10.9308797191587,-5.36989941848476));
#31454=CARTESIAN_POINT('Ctrl Pts',(23.3074042205792,10.9040273043179,-5.39309634457922));
#31455=CARTESIAN_POINT('Ctrl Pts',(23.30346517068,10.8770713907852,-5.41638267982072));
#31456=CARTESIAN_POINT('Ctrl Pts',(23.2997336333505,10.848882976181,-5.43822158177815));
#31457=CARTESIAN_POINT('Ctrl Pts',(23.2962301041906,10.8195249341998,-5.45854814492751));
#31458=CARTESIAN_POINT('Ctrl Pts',(23.2927848639698,10.7906553280341,-5.47853653084243));
#31459=CARTESIAN_POINT('Ctrl Pts',(23.2895600909155,10.760654353199,-5.4970643835706));
#31460=CARTESIAN_POINT('Ctrl Pts',(23.2865740508111,10.7295333552622,-5.51406121620227));
#31461=CARTESIAN_POINT('Ctrl Pts',(23.2852810893787,10.7160578999222,-5.52142087926696));
#31462=CARTESIAN_POINT('Ctrl Pts',(23.2840328739702,10.7023718611015,-5.52849320944327));
#31463=CARTESIAN_POINT('Ctrl Pts',(23.2828308238206,10.6884737128611,-5.53527060182817));
#31464=CARTESIAN_POINT('Ctrl Pts',(23.2796513882161,10.651712960936,-5.55319687774997));
#31465=CARTESIAN_POINT('Ctrl Pts',(23.2768360680739,10.613957098551,-5.56881717513421));
#31466=CARTESIAN_POINT('Ctrl Pts',(23.2743989088803,10.5754946947789,-5.58205636128825));
#31467=CARTESIAN_POINT('Ctrl Pts',(23.2717761315175,10.534102929237,-5.59630386626739));
#31468=CARTESIAN_POINT('Ctrl Pts',(23.2695912980638,10.4918935334026,-5.60779509139924));
#31469=CARTESIAN_POINT('Ctrl Pts',(23.2678586014804,10.4491858295028,-5.61648196879886));
#31470=CARTESIAN_POINT('Ctrl Pts',(23.2658148688682,10.3988116739294,-5.62672822588172));
#31471=CARTESIAN_POINT('Ctrl Pts',(23.2644002050124,10.3477442606575,-5.63307519284311));
#31472=CARTESIAN_POINT('Ctrl Pts',(23.2636332080651,10.2964436468988,-5.63547537799447));
#31473=CARTESIAN_POINT('Ctrl Pts',(23.2627671972425,10.2385204871235,-5.63818541005504));
#31474=CARTESIAN_POINT('Ctrl Pts',(23.2627268559077,10.1802948065651,-5.6358667359521));
#31475=CARTESIAN_POINT('Ctrl Pts',(23.263533211117,10.1223923511815,-5.62843902127006));
#31476=CARTESIAN_POINT('Ctrl Pts',(23.2639716357771,10.0909101160187,-5.62440048682808));
#31477=CARTESIAN_POINT('Ctrl Pts',(23.2646602673992,10.0595233230311,-5.61885097568868));
#31478=CARTESIAN_POINT('Ctrl Pts',(23.2656019440501,10.0283395999061,-5.61177455446721));
#31479=CARTESIAN_POINT('Ctrl Pts',(23.2671983896221,9.9754731338505,-5.59977773866687));
#31480=CARTESIAN_POINT('Ctrl Pts',(23.2695177971326,9.92399532300883,-5.58357606216729));
#31481=CARTESIAN_POINT('Ctrl Pts',(23.2724837537471,9.87434129489678,-5.56346581344797));
#31482=CARTESIAN_POINT('Ctrl Pts',(23.2757491971577,9.8196734625647,-5.54132493692807));
#31483=CARTESIAN_POINT('Ctrl Pts',(23.2797981050074,9.76721027632258,-5.5144435673829));
#31484=CARTESIAN_POINT('Ctrl Pts',(23.2845403622107,9.71751468618776,-5.48319085666352));
#31485=CARTESIAN_POINT('Ctrl Pts',(23.2883092109327,9.6780197466803,-5.45835316148862));
#31486=CARTESIAN_POINT('Ctrl Pts',(23.2925161983746,9.64027247638029,-5.43075214175497));
#31487=CARTESIAN_POINT('Ctrl Pts',(23.2971222524907,9.6045799202608,-5.40059475332545));
#31488=CARTESIAN_POINT('Ctrl Pts',(23.3011856691105,9.57309229070155,-5.37399019544048));
#31489=CARTESIAN_POINT('Ctrl Pts',(23.3055597211743,9.54320452924303,-5.34539527966766));
#31490=CARTESIAN_POINT('Ctrl Pts',(23.3102215256331,9.5151437081236,-5.31498951086506));
#31491=CARTESIAN_POINT('Ctrl Pts',(23.3129951951883,9.49844814615341,-5.29689875738589));
#31492=CARTESIAN_POINT('Ctrl Pts',(23.3158708013444,9.48239961855491,-5.27816776321047));
#31493=CARTESIAN_POINT('Ctrl Pts',(23.3188442014171,9.46704699216216,-5.25884324386485));
#31494=CARTESIAN_POINT('Ctrl Pts',(23.3227492502484,9.44688396186458,-5.23346381632692));
#31495=CARTESIAN_POINT('Ctrl Pts',(23.3267744375398,9.4281134250268,-5.20731048454305));
#31496=CARTESIAN_POINT('Ctrl Pts',(23.3309114958432,9.41068440947216,-5.18040132771481));
#31497=CARTESIAN_POINT('Ctrl Pts',(23.3350828281238,9.3931110010575,-5.15326923861005));
#31498=CARTESIAN_POINT('Ctrl Pts',(23.3393678806161,9.37690163249573,-5.1253670769023));
#31499=CARTESIAN_POINT('Ctrl Pts',(23.3437589204372,9.36205724353143,-5.09671411485491));
#31500=CARTESIAN_POINT('Ctrl Pts',(23.3481443762077,9.34723173205895,-5.06809759055231));
#31501=CARTESIAN_POINT('Ctrl Pts',(23.3526355376376,9.33376849043178,-5.03873076660441));
#31502=CARTESIAN_POINT('Ctrl Pts',(23.35722562536,9.32171392291677,-5.00865683320089));
#31503=CARTESIAN_POINT('Ctrl Pts',(23.3593782227678,9.31606073449098,-4.9945531656887));
#31504=CARTESIAN_POINT('Ctrl Pts',(23.3615525914125,9.31071793545332,-4.98029445988451));
#31505=CARTESIAN_POINT('Ctrl Pts',(23.3637481126768,9.30569287797804,-4.96588820382791));
#31506=CARTESIAN_POINT('Ctrl Pts',(23.3688944674221,9.29391402217532,-4.93211959250706));
#31507=CARTESIAN_POINT('Ctrl Pts',(23.3741025072454,9.28400173534217,-4.89789163347882));
#31508=CARTESIAN_POINT('Ctrl Pts',(23.3793475390172,9.27594399955006,-4.86331291591488));
#31509=CARTESIAN_POINT('Ctrl Pts',(23.3845745401648,9.26791396349586,-4.82885306814737));
#31510=CARTESIAN_POINT('Ctrl Pts',(23.3898383021294,9.26172758375133,-4.79404408151541));
#31511=CARTESIAN_POINT('Ctrl Pts',(23.395115005992,9.2573942639056,-4.75904010029301));
#31512=CARTESIAN_POINT('Ctrl Pts',(23.4003235118704,9.25311694941585,-4.72448852288534));
#31513=CARTESIAN_POINT('Ctrl Pts',(23.4055446650074,9.25064690350392,-4.68974712944241));
#31514=CARTESIAN_POINT('Ctrl Pts',(23.4107557118458,9.24998669647212,-4.65501404155883));
#31515=CARTESIAN_POINT('Ctrl Pts',(23.411657828817,9.24987240389592,-4.64900117907418));
#31516=CARTESIAN_POINT('Ctrl Pts',(23.4125596424264,9.24981229765042,-4.6429886806042));
#31517=CARTESIAN_POINT('Ctrl Pts',(23.4134610336593,9.24980631172449,-4.63697771374339));
#31518=CARTESIAN_POINT('Ctrl Pts',(23.7407619571655,9.2417425355196,-4.76017122167868));
#31519=CARTESIAN_POINT('Ctrl Pts',(22.2581052131567,9.30443264497317,-8.73250381527275));
#31520=CARTESIAN_POINT('Ctrl Pts',(23.66457973822,11.1412914989991,-5.17871622099501));
#31521=CARTESIAN_POINT('Ctrl Pts',(23.5838527574288,9.24837701443423,-4.69515805555824));
#31522=CARTESIAN_POINT('Ctrl Pts',(22.1715287485385,9.28227205649985,-8.80903324352776));
#31523=CARTESIAN_POINT('Ctrl Pts',(23.490707426048,11.1509430734207,-5.10875525275042));
#31524=CARTESIAN_POINT('Ctrl Pts',(23.4236136142519,9.25115309215875,-4.63708387423802));
#31525=CARTESIAN_POINT('Ctrl Pts',(22.1106313281463,9.25892841933612,-8.89170684279919));
#31526=CARTESIAN_POINT('Ctrl Pts',(23.3131450879115,11.1559910950577,-5.04633195118703));
#31527=CARTESIAN_POINT('Ctrl Pts',(23.0965052560008,9.2479723676883,-4.53914929014038));
#31528=CARTESIAN_POINT('Ctrl Pts',(22.0406305439231,9.21636517829358,-9.05096883883774));
#31529=CARTESIAN_POINT('Ctrl Pts',(22.9506736640093,11.1556438435962,-4.94129943123646));
#31530=CARTESIAN_POINT('Ctrl Pts',(22.9322244640352,9.24204169116783,-4.50009212968019));
#31531=CARTESIAN_POINT('Ctrl Pts',(22.0347031030604,9.1981366813795,-9.12437043488707));
#31532=CARTESIAN_POINT('Ctrl Pts',(22.7686327863313,11.1502523788117,-4.89955233099308));
#31533=CARTESIAN_POINT('Ctrl Pts',(22.601998284174,9.22119105391794,-4.44398991580241));
#31534=CARTESIAN_POINT('Ctrl Pts',(22.0626396540039,9.17409017957756,-9.23227690113227));
#31535=CARTESIAN_POINT('Ctrl Pts',(22.4027064790007,11.1286492452038,-4.84001519960698));
#31536=CARTESIAN_POINT('Ctrl Pts',(22.4360515375488,9.2062707034032,-4.42695779702948));
#31537=CARTESIAN_POINT('Ctrl Pts',(22.0969461288735,9.168883245967,-9.26448307520217));
#31538=CARTESIAN_POINT('Ctrl Pts',(22.2188195434826,11.1124371401094,-4.82223930830889));
#31539=CARTESIAN_POINT('Ctrl Pts',(22.1023644694404,9.16701301620337,-4.41641652003192));
#31540=CARTESIAN_POINT('Ctrl Pts',(22.1690030235667,9.17234315197961,-9.26969035127475));
#31541=CARTESIAN_POINT('Ctrl Pts',(21.8490581977948,11.0686622585437,-4.81232681866023));
#31542=CARTESIAN_POINT('Ctrl Pts',(21.9335430214035,9.14244254294621,-4.42314440604185));
#31543=CARTESIAN_POINT('Ctrl Pts',(22.2054462396773,9.18107611879875,-9.24187069747537));
#31544=CARTESIAN_POINT('Ctrl Pts',(21.661985782483,11.0408296166206,-4.82045399638167));
#31545=CARTESIAN_POINT('Ctrl Pts',(21.6031838656795,9.08511086427486,-4.45915125113957));
#31546=CARTESIAN_POINT('Ctrl Pts',(22.2377167051826,9.20360768905055,-9.13809050812787));
#31547=CARTESIAN_POINT('Ctrl Pts',(21.2959121232227,10.9751791255569,-4.86128347077255));
#31548=CARTESIAN_POINT('Ctrl Pts',(21.4408293418957,9.05231840460623,-4.48822269433724));
#31549=CARTESIAN_POINT('Ctrl Pts',(22.2341132638195,9.21686200399614,-9.06491957153717));
#31550=CARTESIAN_POINT('Ctrl Pts',(21.1160057592652,10.9373324408439,-4.89376350993861));
#31551=CARTESIAN_POINT('Ctrl Pts',(21.1211096105402,8.97894474489699,-4.56528168833185));
#31552=CARTESIAN_POINT('Ctrl Pts',(22.1702544220307,9.23658596371069,-8.90266922033884));
#31553=CARTESIAN_POINT('Ctrl Pts',(20.761721732372,10.8521500222688,-4.97937766766415));
#31554=CARTESIAN_POINT('Ctrl Pts',(20.9637426859415,8.93836248783126,-4.61325801902883));
#31555=CARTESIAN_POINT('Ctrl Pts',(22.1126646934585,9.2430926653662,-8.815604632918));
#31556=CARTESIAN_POINT('Ctrl Pts',(20.5873421675309,10.8048130510551,-5.03249953644066));
#31557=CARTESIAN_POINT('Ctrl Pts',(20.6533775196975,8.84967655519081,-4.72488961260549));
#31558=CARTESIAN_POINT('Ctrl Pts',(21.9467029793221,9.24171267207773,-8.65176604079951));
#31559=CARTESIAN_POINT('Ctrl Pts',(20.2434240100882,10.7009666613119,-5.15589424043288));
#31560=CARTESIAN_POINT('Ctrl Pts',(20.5017967315099,8.80196327630676,-4.78803948205891));
#31561=CARTESIAN_POINT('Ctrl Pts',(21.8422688128588,9.23443217585936,-8.5761898974068));
#31562=CARTESIAN_POINT('Ctrl Pts',(20.0754561099999,10.644913701976,-5.22560855463383));
#31563=CARTESIAN_POINT('Ctrl Pts',(20.2067132658722,8.70095212509222,-4.92446247464717));
#31564=CARTESIAN_POINT('Ctrl Pts',(21.6025383820459,9.20382388721751,-8.4499513783311));
#31565=CARTESIAN_POINT('Ctrl Pts',(19.7484717287398,10.5259271136452,-5.37612047005189));
#31566=CARTESIAN_POINT('Ctrl Pts',(20.0627946620671,8.64753209592579,-4.99789368139045));
#31567=CARTESIAN_POINT('Ctrl Pts',(21.4693310632381,9.18140104347433,-8.39815497287525));
#31568=CARTESIAN_POINT('Ctrl Pts',(19.5889943573367,10.4628503478549,-5.45709259294587));
#31569=CARTESIAN_POINT('Ctrl Pts',(19.6399435274182,8.47880310571364,-5.22981959670209));
#31570=CARTESIAN_POINT('Ctrl Pts',(21.0540930964424,9.09375652030717,-8.28451329894513));
#31571=CARTESIAN_POINT('Ctrl Pts',(19.1204295859944,10.2632105486208,-5.71278462460776));
#31572=CARTESIAN_POINT('Ctrl Pts',(19.3697981552916,8.35506889938905,-5.39973069152153));
#31573=CARTESIAN_POINT('Ctrl Pts',(20.7428055844105,9.00839665528852,-8.25231835531753));
#31574=CARTESIAN_POINT('Ctrl Pts',(18.8210793093145,10.1162920672119,-5.9000462023183));
#31575=CARTESIAN_POINT('Ctrl Pts',(18.8465231014693,8.0850404366681,-5.75593885943587));
#31576=CARTESIAN_POINT('Ctrl Pts',(20.1091011680343,8.78661111089581,-8.27115731644347));
#31577=CARTESIAN_POINT('Ctrl Pts',(18.2412339790073,9.79473667310455,-6.29272730255182));
#31578=CARTESIAN_POINT('Ctrl Pts',(18.5933272070726,7.93849035974423,-5.94254947324762));
#31579=CARTESIAN_POINT('Ctrl Pts',(19.7883641219259,8.65484775926693,-8.31467161177097));
#31580=CARTESIAN_POINT('Ctrl Pts',(17.9606655558799,9.61978930542312,-6.49849119520135));
#31581=CARTESIAN_POINT('Ctrl Pts',(18.108340600348,7.62696348416377,-6.31757114103161));
#31582=CARTESIAN_POINT('Ctrl Pts',(19.1687148199052,8.35509365521475,-8.4508622545085));
#31583=CARTESIAN_POINT('Ctrl Pts',(17.4232479642539,9.24709047831589,-6.91219203660589));
#31584=CARTESIAN_POINT('Ctrl Pts',(17.8754091113951,7.46141940260319,-6.5068329586448));
#31585=CARTESIAN_POINT('Ctrl Pts',(18.8667622645576,8.18964072402686,-8.53948871553438));
#31586=CARTESIAN_POINT('Ctrl Pts',(17.1651346929798,9.04866437084577,-7.12106524937581));
#31587=CARTESIAN_POINT('Ctrl Pts',(17.4259063892177,7.10978479208954,-6.88361837145848));
#31588=CARTESIAN_POINT('Ctrl Pts',(18.2867484113725,7.82705740885029,-8.74367560464804));
#31589=CARTESIAN_POINT('Ctrl Pts',(16.6670370817724,8.62645478348271,-7.53711266367819));
#31590=CARTESIAN_POINT('Ctrl Pts',(17.2093611002873,6.92369688326685,-7.0711829314943));
#31591=CARTESIAN_POINT('Ctrl Pts',(18.0064015521297,7.63180988067425,-8.85753153715041));
#31592=CARTESIAN_POINT('Ctrl Pts',(16.4270814913594,8.40267421479281,-7.74433143391629));
#31593=CARTESIAN_POINT('Ctrl Pts',(16.7915601485188,6.52931017355786,-7.44095042941296));
#31594=CARTESIAN_POINT('Ctrl Pts',(17.4699776474557,7.21116075749424,-9.09855744937918));
#31595=CARTESIAN_POINT('Ctrl Pts',(15.9641128692286,7.92771133699107,-8.15307202858187));
#31596=CARTESIAN_POINT('Ctrl Pts',(16.5903133615341,6.32102030483416,-7.62317736202818));
#31597=CARTESIAN_POINT('Ctrl Pts',(17.2117049676949,6.98709902479069,-9.22521672502677));
#31598=CARTESIAN_POINT('Ctrl Pts',(15.7411096725996,7.67653975440558,-8.35462007956716));
#31599=CARTESIAN_POINT('Ctrl Pts',(16.2031446806553,5.87972109786976,-7.9792052599084));
#31600=CARTESIAN_POINT('Ctrl Pts',(16.7193587393204,6.50795989920566,-9.48276769470842));
#31601=CARTESIAN_POINT('Ctrl Pts',(15.3120849184942,7.14371633451588,-8.74861548265883));
#31602=CARTESIAN_POINT('Ctrl Pts',(16.0164899333278,5.64553819281045,-8.15373034271471));
#31603=CARTESIAN_POINT('Ctrl Pts',(16.482150418559,6.25235099264002,-9.61448883029963));
#31604=CARTESIAN_POINT('Ctrl Pts',(15.1052512793004,6.86064228488974,-8.94186563738397));
#31605=CARTESIAN_POINT('Ctrl Pts',(15.4909684360467,4.91507969565495,-8.65057793645775));
#31606=CARTESIAN_POINT('Ctrl Pts',(15.8360790816217,5.47002026758944,-9.98913906363838));
#31607=CARTESIAN_POINT('Ctrl Pts',(14.5229166473954,5.97672576172198,-9.49231103543021));
#31608=CARTESIAN_POINT('Ctrl Pts',(15.1832050299975,4.38890092270191,-8.94897579566626));
#31609=CARTESIAN_POINT('Ctrl Pts',(15.4437153305843,4.88646935114675,-10.2366313764018));
#31610=CARTESIAN_POINT('Ctrl Pts',(14.1818815208225,5.33879252138579,-9.82330325380897));
#31611=CARTESIAN_POINT('Ctrl Pts',(14.7936282028206,3.52847339741587,-9.33030908404118));
#31612=CARTESIAN_POINT('Ctrl Pts',(14.953492875312,3.91856318300104,-10.5580046380276));
#31613=CARTESIAN_POINT('Ctrl Pts',(13.7501882811056,4.29397409879376,-10.2466106841205));
#31614=CARTESIAN_POINT('Ctrl Pts',(14.6754746649165,3.2278437718719,-9.44675123187285));
#31615=CARTESIAN_POINT('Ctrl Pts',(14.8068781272224,3.58487283062697,-10.656336839848));
#31616=CARTESIAN_POINT('Ctrl Pts',(13.6192613872657,3.92866298901994,-10.3759324896199));
#31617=CARTESIAN_POINT('Ctrl Pts',(14.4718580234029,2.61628749337707,-9.6481638527312));
#31618=CARTESIAN_POINT('Ctrl Pts',(14.5564895360256,2.9071846621386,-10.8265016627336));
#31619=CARTESIAN_POINT('Ctrl Pts',(13.3936321360263,3.185098162674,-10.5996927978589));
#31620=CARTESIAN_POINT('Ctrl Pts',(14.3855728281781,2.3039822459725,-9.73393618883941));
#31621=CARTESIAN_POINT('Ctrl Pts',(14.4498967803323,2.55973319778683,-10.9001427667305));
#31622=CARTESIAN_POINT('Ctrl Pts',(13.2980188112511,2.8051729619165,-10.6950206797896));
#31623=CARTESIAN_POINT('Ctrl Pts',(14.2453335983135,1.66563454054454,-9.87363041164593));
#31624=CARTESIAN_POINT('Ctrl Pts',(14.2781912174048,1.8516228470949,-11.0196358705889));
#31625=CARTESIAN_POINT('Ctrl Pts',(13.1426185840695,2.02830937336854,-10.8503077377617));
#31626=CARTESIAN_POINT('Ctrl Pts',(14.1913682276192,1.33959736847006,-9.92756592003646));
#31627=CARTESIAN_POINT('Ctrl Pts',(14.211738551509,1.48849006021389,-11.0663999130354));
#31628=CARTESIAN_POINT('Ctrl Pts',(13.0828191185393,1.63137711985507,-10.910281907528));
#31629=CARTESIAN_POINT('Ctrl Pts',(14.1183867686561,0.672587688372933,-10.0005590742266));
#31630=CARTESIAN_POINT('Ctrl Pts',(14.1226151474584,0.748193939568345,-11.1292768460617));
#31631=CARTESIAN_POINT('Ctrl Pts',(13.0019477730282,0.819164813667982,-10.9914533471288));
#31632=CARTESIAN_POINT('Ctrl Pts',(14.10005646014,0.335334215738292,-10.0189290741656));
#31633=CARTESIAN_POINT('Ctrl Pts',(14.1000688879279,0.372241137368051,-11.1452899367182));
#31634=CARTESIAN_POINT('Ctrl Pts',(12.981635809193,0.408413807466937,-11.0118855214374));
#31635=CARTESIAN_POINT('Ctrl Pts',(14.0999438033074,-0.332212108254802,
-10.019041900077));
#31636=CARTESIAN_POINT('Ctrl Pts',(14.0999314344141,-0.368770536470457,
-11.1453873481658));
#31637=CARTESIAN_POINT('Ctrl Pts',(12.9815109730246,-0.404611297179373,
-11.0120110046255));
#31638=CARTESIAN_POINT('Ctrl Pts',(14.1179004591993,-0.664694731558155,
-10.0010464561665));
#31639=CARTESIAN_POINT('Ctrl Pts',(14.1220155872155,-0.739394626095605,
-11.1297027095952));
#31640=CARTESIAN_POINT('Ctrl Pts',(13.0014088890623,-0.809551999095349,
-10.9919954420619));
#31641=CARTESIAN_POINT('Ctrl Pts',(14.1896347468004,-1.32709812952424,-9.92929871441566));
#31642=CARTESIAN_POINT('Ctrl Pts',(14.2096143866203,-1.47458064058229,-11.0678957127947));
#31643=CARTESIAN_POINT('Ctrl Pts',(13.0808982349024,-1.61615847282446,-10.9122087447037));
#31644=CARTESIAN_POINT('Ctrl Pts',(14.2440819345987,-1.65935479644565,-9.87487858129904));
#31645=CARTESIAN_POINT('Ctrl Pts',(14.2766700735661,-1.84470377647724,-11.0206983934546));
#31646=CARTESIAN_POINT('Ctrl Pts',(13.1412316055102,-2.02066592075089,-10.8516953675167));
#31647=CARTESIAN_POINT('Ctrl Pts',(14.4559527871627,-2.62549667548358,-9.66382702633439));
#31648=CARTESIAN_POINT('Ctrl Pts',(14.5383068586704,-2.92564928123915,-10.838608544174));
#31649=CARTESIAN_POINT('Ctrl Pts',(13.3760074138938,-3.19645531868435,-10.6170855755652));
#31650=CARTESIAN_POINT('Ctrl Pts',(14.6610301802517,-3.23529958684364,-9.46010767782022));
#31651=CARTESIAN_POINT('Ctrl Pts',(14.797274385157,-3.6097730509549,-10.6604338378256));
#31652=CARTESIAN_POINT('Ctrl Pts',(13.6032553377581,-3.9379706819944,-10.3906969750855));
#31653=CARTESIAN_POINT('Ctrl Pts',(15.1843845801438,-4.39182021036076,-8.94781484699701));
#31654=CARTESIAN_POINT('Ctrl Pts',(15.4453374658606,-4.89004382349708,-10.2355491633465));
#31655=CARTESIAN_POINT('Ctrl Pts',(14.1831885897263,-5.34233943366017,-9.82201402046962));
#31656=CARTESIAN_POINT('Ctrl Pts',(15.4928501358146,-4.91768382207714,-8.64879979303374));
#31657=CARTESIAN_POINT('Ctrl Pts',(15.8382253403148,-5.47260629285237,-9.98789683284872));
#31658=CARTESIAN_POINT('Ctrl Pts',(14.5250017742756,-5.97987683694916,-9.49034111898627));
#31659=CARTESIAN_POINT('Ctrl Pts',(16.0154588429638,-5.64411069667211,-8.15470473125201));
#31660=CARTESIAN_POINT('Ctrl Pts',(16.4807916124111,-6.25071253065397,-9.61527551915532));
#31661=CARTESIAN_POINT('Ctrl Pts',(15.1041087196526,-6.8589149628141,-8.94294511605303));
#31662=CARTESIAN_POINT('Ctrl Pts',(16.1997926205015,-5.87571307364266,-7.98231314503237));
#31663=CARTESIAN_POINT('Ctrl Pts',(16.7151650787374,-6.50365717348269,-9.48502957169505));
#31664=CARTESIAN_POINT('Ctrl Pts',(15.3083704732675,-7.13887424906056,-8.75205577992599));
#31665=CARTESIAN_POINT('Ctrl Pts',(16.5885891387386,-6.31923989565411,-7.62473779388686));
#31666=CARTESIAN_POINT('Ctrl Pts',(17.2095626811808,-6.98524577388381,-9.2262661640785));
#31667=CARTESIAN_POINT('Ctrl Pts',(15.7391990475312,-7.67439286523923,-8.35634595037217));
#31668=CARTESIAN_POINT('Ctrl Pts',(16.7921363319381,-6.52995311691278,-7.44041803646221));
#31669=CARTESIAN_POINT('Ctrl Pts',(17.4708015184657,-7.21192656737724,-9.0981285045576));
#31670=CARTESIAN_POINT('Ctrl Pts',(15.9647513427821,-7.92848739989083,-8.15248290996759));
#31671=CARTESIAN_POINT('Ctrl Pts',(17.2121549286183,-6.92623429272213,-7.06873293473742));
#31672=CARTESIAN_POINT('Ctrl Pts',(18.0100906225307,-7.63457381075248,-8.85593723561199));
#31673=CARTESIAN_POINT('Ctrl Pts',(16.4301773551509,-8.40572826049159,-7.74162382709166));
#31674=CARTESIAN_POINT('Ctrl Pts',(17.4293842420214,-7.11268557699717,-6.88063705161154));
#31675=CARTESIAN_POINT('Ctrl Pts',(18.2912497012959,-7.83009389817568,-8.7419225173432));
#31676=CARTESIAN_POINT('Ctrl Pts',(16.6708909186913,-8.62994147543376,-7.53381951966801));
#31677=CARTESIAN_POINT('Ctrl Pts',(17.8792347652403,-7.46422901691747,-6.50369336197627));
#31678=CARTESIAN_POINT('Ctrl Pts',(18.8717133714707,-8.19249183101686,-8.53793037040513));
#31679=CARTESIAN_POINT('Ctrl Pts',(17.1693739309962,-9.05203412564116,-7.11759968080442));
#31680=CARTESIAN_POINT('Ctrl Pts',(18.1118335517547,-7.62931683180686,-6.31480630165245));
#31681=CARTESIAN_POINT('Ctrl Pts',(19.1730958355485,-8.35735093042499,-8.44974107184639));
#31682=CARTESIAN_POINT('Ctrl Pts',(17.4271185320558,-9.24990851491713,-6.9091414254315));
#31683=CARTESIAN_POINT('Ctrl Pts',(18.5948661394437,-7.9393680496501,-5.94142401732326));
#31684=CARTESIAN_POINT('Ctrl Pts',(19.7901868370082,-8.6555775096822,-8.31444537841736));
#31685=CARTESIAN_POINT('Ctrl Pts',(17.9623708592913,-9.62083673142101,-6.49725027823761));
#31686=CARTESIAN_POINT('Ctrl Pts',(18.8452448672861,-8.08433603821065,-5.7568497334406));
#31687=CARTESIAN_POINT('Ctrl Pts',(20.1075342963327,-8.78600595448993,-8.27130268715703));
#31688=CARTESIAN_POINT('Ctrl Pts',(18.239817557234,-9.79389664474636,-6.29373156030851));
#31689=CARTESIAN_POINT('Ctrl Pts',(19.3688604852375,-8.35462962365301,-5.40032841845693));
#31690=CARTESIAN_POINT('Ctrl Pts',(20.7417386093025,-9.00808560232857,-8.25224155607797));
#31691=CARTESIAN_POINT('Ctrl Pts',(18.8200402696357,-10.1157701798982,-5.90070501493886));
#31692=CARTESIAN_POINT('Ctrl Pts',(19.6422136178767,-8.47984841605453,-5.2283819419454));
#31693=CARTESIAN_POINT('Ctrl Pts',(21.0568753448171,-9.09452026307236,-8.28480003990359));
#31694=CARTESIAN_POINT('Ctrl Pts',(19.1229450916605,-10.26445186785,-5.71120023558755));
#31695=CARTESIAN_POINT('Ctrl Pts',(20.0671700727504,-8.64920689557343,-4.99559201149219));
#31696=CARTESIAN_POINT('Ctrl Pts',(21.4735709337441,-9.18219869325014,-8.39957693279326));
#31697=CARTESIAN_POINT('Ctrl Pts',(19.5938427853797,-10.4648296682004,-5.45455476540464));
#31698=CARTESIAN_POINT('Ctrl Pts',(20.2116262715113,-8.70273072020049,-4.92202982910422));
#31699=CARTESIAN_POINT('Ctrl Pts',(21.6069299528932,-9.20451236245352,-8.45183085092374));
#31700=CARTESIAN_POINT('Ctrl Pts',(19.7539158701371,-10.528025719249,-5.37343760461358));
#31701=CARTESIAN_POINT('Ctrl Pts',(20.5073293440887,-8.80375687931068,-4.78564870666182));
#31702=CARTESIAN_POINT('Ctrl Pts',(21.8463416500992,-9.23481277781289,-8.57880710613263));
#31703=CARTESIAN_POINT('Ctrl Pts',(20.0815868428442,-10.6470228590782,-5.22296982983514));
#31704=CARTESIAN_POINT('Ctrl Pts',(20.6587941143368,-8.8513250187248,-4.72274331597064));
#31705=CARTESIAN_POINT('Ctrl Pts',(21.950144168652,-9.24188863040543,-8.65453053690068));
#31706=CARTESIAN_POINT('Ctrl Pts',(20.2494261825329,-10.702901113401,-5.15352385726253));
#31707=CARTESIAN_POINT('Ctrl Pts',(20.9691881873021,-8.93981424967264,-4.61150450922749));
#31708=CARTESIAN_POINT('Ctrl Pts',(22.1149730983979,-9.24295181576889,-8.81857069716009));
#31709=CARTESIAN_POINT('Ctrl Pts',(20.5933763717348,-10.8065086445252,-5.03055909951977));
#31710=CARTESIAN_POINT('Ctrl Pts',(21.1264314986761,-8.98025816049582,-4.56379204973175));
#31711=CARTESIAN_POINT('Ctrl Pts',(22.1718570677214,-9.2363230349133,-8.90552485176888));
#31712=CARTESIAN_POINT('Ctrl Pts',(20.7676189597731,-10.8536794210946,-4.97772638126974));
#31713=CARTESIAN_POINT('Ctrl Pts',(21.4455519698772,-9.05330719736127,-4.48729801630187));
#31714=CARTESIAN_POINT('Ctrl Pts',(22.2344681686058,-9.21650383205574,-9.06712395562859));
#31715=CARTESIAN_POINT('Ctrl Pts',(21.1212389416158,-10.9384756207102,-4.89273232060626));
#31716=CARTESIAN_POINT('Ctrl Pts',(21.6074307679876,-9.08591315593356,-4.4585279467887));
#31717=CARTESIAN_POINT('Ctrl Pts',(22.2375705897678,-9.20328697843773,-9.13973863765263));
#31718=CARTESIAN_POINT('Ctrl Pts',(21.3006181501117,-10.9761020130789,-4.86058352992028));
#31719=CARTESIAN_POINT('Ctrl Pts',(21.9363949761706,-9.14287078778472,-4.42299748379683));
#31720=CARTESIAN_POINT('Ctrl Pts',(22.2048926812382,-9.18091771620324,-9.24242200205805));
#31721=CARTESIAN_POINT('Ctrl Pts',(21.6651460566772,-11.0413157248983,-4.82028039988043));
#31722=CARTESIAN_POINT('Ctrl Pts',(22.1048907604966,-9.16736445942107,-4.41635803485168));
#31723=CARTESIAN_POINT('Ctrl Pts',(22.1684501645743,-9.17223852797182,-9.26999463874004));
#31724=CARTESIAN_POINT('Ctrl Pts',(21.8518576014085,-11.0690591488402,-4.8122511790867));
#31725=CARTESIAN_POINT('Ctrl Pts',(22.4394530739544,-9.206615689037,-4.42720601632188));
#31726=CARTESIAN_POINT('Ctrl Pts',(22.0962240073149,-9.16892796897462,-9.26408083371504));
#31727=CARTESIAN_POINT('Ctrl Pts',(22.2225888135429,-11.1128167238586,-4.82249373339013));
#31728=CARTESIAN_POINT('Ctrl Pts',(22.6053470679695,-9.22145320686374,-4.44443202209375));
#31729=CARTESIAN_POINT('Ctrl Pts',(22.0621296126529,-9.17426072073414,-9.23141868494471));
#31730=CARTESIAN_POINT('Ctrl Pts',(22.4064172934819,-11.1289294582834,-4.84048097506774));
#31731=CARTESIAN_POINT('Ctrl Pts',(22.9345901710377,-9.24213946603061,-4.50062308032295));
#31732=CARTESIAN_POINT('Ctrl Pts',(22.0347284941016,-9.19838211472973,-9.1233615918879));
#31733=CARTESIAN_POINT('Ctrl Pts',(22.771254245437,-11.1503449327046,-4.90011924842924));
#31734=CARTESIAN_POINT('Ctrl Pts',(23.0979412457337,-9.24798849555332,-4.53957417540497));
#31735=CARTESIAN_POINT('Ctrl Pts',(22.0409347063402,-9.21655719993794,-9.05024798954247));
#31736=CARTESIAN_POINT('Ctrl Pts',(22.9522648958751,-11.1556479741126,-4.94175504041852));
#31737=CARTESIAN_POINT('Ctrl Pts',(23.4224245118462,-9.25113936332021,-4.6367329096279));
#31738=CARTESIAN_POINT('Ctrl Pts',(22.1104006734227,-9.25878135062781,-8.89225940304983));
#31739=CARTESIAN_POINT('Ctrl Pts',(23.3118274338947,-11.1559872246472,-5.04595562020784));
#31740=CARTESIAN_POINT('Ctrl Pts',(23.5842228676575,-9.24836752493948,-4.69529858884187));
#31741=CARTESIAN_POINT('Ctrl Pts',(22.1715953285364,-9.28230057369568,-8.80893197595439));
#31742=CARTESIAN_POINT('Ctrl Pts',(23.4911181003785,-11.1509276833783,-5.10890659395469));
#31743=CARTESIAN_POINT('Ctrl Pts',(23.7411245379554,-9.24172719765138,-4.76032146685216));
#31744=CARTESIAN_POINT('Ctrl Pts',(22.2583006396915,-9.30448265446957,-8.73233111548978));
#31745=CARTESIAN_POINT('Ctrl Pts',(23.6649815169331,-11.1412691878794,-5.17887790068865));
#31746=CARTESIAN_POINT('Ctrl Pts',(23.3608103941008,-11.1532440216953,-5.06593335958171));
#31747=CARTESIAN_POINT('Ctrl Pts',(23.3559722305032,-11.138804320256,-5.09632894678172));
#31748=CARTESIAN_POINT('Ctrl Pts',(23.3512065153187,-11.1228190011423,-5.12599866299092));
#31749=CARTESIAN_POINT('Ctrl Pts',(23.3465578204016,-11.1054052152928,-5.15474249120358));
#31750=CARTESIAN_POINT('Ctrl Pts',(23.3418303981347,-11.0876965206065,-5.18397310666727));
#31751=CARTESIAN_POINT('Ctrl Pts',(23.337224112825,-11.0685120446219,-5.21224603668186));
#31752=CARTESIAN_POINT('Ctrl Pts',(23.3327737836655,-11.047987014281,-5.23940280567959));
#31753=CARTESIAN_POINT('Ctrl Pts',(23.3282422691374,-11.0270875549723,-5.26705498349359));
#31754=CARTESIAN_POINT('Ctrl Pts',(23.3238723870196,-11.0047996898859,-5.29355036578414));
#31755=CARTESIAN_POINT('Ctrl Pts',(23.3196880352788,-10.9812554009882,-5.31877288978583));
#31756=CARTESIAN_POINT('Ctrl Pts',(23.315387879271,-10.9570595107707,-5.34469346119934));
#31757=CARTESIAN_POINT('Ctrl Pts',(23.311283395679,-10.9315380356051,-5.36927083384139));
#31758=CARTESIAN_POINT('Ctrl Pts',(23.3073895706749,-10.9048005533827,-5.39242091162555));
#31759=CARTESIAN_POINT('Ctrl Pts',(23.3034822287278,-10.8779702552219,-5.4156513521072));
#31760=CARTESIAN_POINT('Ctrl Pts',(23.2997865168957,-10.8499161036061,-5.43744630453823));
#31761=CARTESIAN_POINT('Ctrl Pts',(23.2963126014671,-10.8207004597727,-5.45774050941342));
#31762=CARTESIAN_POINT('Ctrl Pts',(23.2928965023705,-10.7919710515426,-5.47769695808488));
#31763=CARTESIAN_POINT('Ctrl Pts',(23.289694322584,-10.7621181834791,-5.49620400088566));
#31764=CARTESIAN_POINT('Ctrl Pts',(23.286718800121,-10.7311525663159,-5.51319208968022));
#31765=CARTESIAN_POINT('Ctrl Pts',(23.2853739925347,-10.7171574453269,-5.52086997179056));
#31766=CARTESIAN_POINT('Ctrl Pts',(23.2840755758007,-10.7029343921086,-5.5282373181478));
#31767=CARTESIAN_POINT('Ctrl Pts',(23.2828254101566,-10.6884815434047,-5.53528569817435));
#31768=CARTESIAN_POINT('Ctrl Pts',(23.279658478254,-10.6518694449539,-5.55314072376397));
#31769=CARTESIAN_POINT('Ctrl Pts',(23.276837945852,-10.6142687495006,-5.5687056045139));
#31770=CARTESIAN_POINT('Ctrl Pts',(23.2743937471177,-10.5759656011028,-5.58190860303003));
#31771=CARTESIAN_POINT('Ctrl Pts',(23.2717710871026,-10.53486577794,-5.5960756082745));
#31772=CARTESIAN_POINT('Ctrl Pts',(23.2695814696403,-10.4929578204317,-5.60752453362935));
#31773=CARTESIAN_POINT('Ctrl Pts',(23.2678450316622,-10.4505558414619,-5.61620955990059));
#31774=CARTESIAN_POINT('Ctrl Pts',(23.2657327548319,-10.3989762752072,-5.62677439434617));
#31775=CARTESIAN_POINT('Ctrl Pts',(23.2642908067166,-10.3466661130416,-5.63325169235027));
#31776=CARTESIAN_POINT('Ctrl Pts',(23.2635352842541,-10.2941199808551,-5.63559065520854));
#31777=CARTESIAN_POINT('Ctrl Pts',(23.2627150161734,-10.2370708299206,-5.63813005895872));
#31778=CARTESIAN_POINT('Ctrl Pts',(23.2627034573345,-10.1797382740423,-5.63579433971693));
#31779=CARTESIAN_POINT('Ctrl Pts',(23.2635073144818,-10.1227172982536,-5.62850315363752));
#31780=CARTESIAN_POINT('Ctrl Pts',(23.2639526948926,-10.091124588397,-5.62446344152928));
#31781=CARTESIAN_POINT('Ctrl Pts',(23.264648241806,-10.0596273344297,-5.61890183621911));
#31782=CARTESIAN_POINT('Ctrl Pts',(23.265593203137,-10.0283334039203,-5.61180069629684));
#31783=CARTESIAN_POINT('Ctrl Pts',(23.2671319225926,-9.97737620796019,-5.6002376176848));
#31784=CARTESIAN_POINT('Ctrl Pts',(23.2692956663857,-9.92770792626252,-5.58475854587693));
#31785=CARTESIAN_POINT('Ctrl Pts',(23.2720642636561,-9.87971988451815,-5.56563891702826));
#31786=CARTESIAN_POINT('Ctrl Pts',(23.2751704015229,-9.82588125828915,-5.54418826987111));
#31787=CARTESIAN_POINT('Ctrl Pts',(23.2790386770644,-9.77415227312768,-5.5181532747369));
#31788=CARTESIAN_POINT('Ctrl Pts',(23.2836179425702,-9.72506586357993,-5.48789049047839));
#31789=CARTESIAN_POINT('Ctrl Pts',(23.2873494782671,-9.68506650358983,-5.46323005976016));
#31790=CARTESIAN_POINT('Ctrl Pts',(23.2915531940299,-9.64682123564115,-5.43575978462185));
#31791=CARTESIAN_POINT('Ctrl Pts',(23.2961824949623,-9.61064170173483,-5.40568734159021));
#31792=CARTESIAN_POINT('Ctrl Pts',(23.3002576043707,-9.5787933597996,-5.37921498705466));
#31793=CARTESIAN_POINT('Ctrl Pts',(23.3046625412563,-9.54854647437181,-5.35072529360372));
#31794=CARTESIAN_POINT('Ctrl Pts',(23.3093483241437,-9.52013037227305,-5.32039252488423));
#31795=CARTESIAN_POINT('Ctrl Pts',(23.312399140962,-9.50162923291665,-5.30064348333047));
#31796=CARTESIAN_POINT('Ctrl Pts',(23.3155686554131,-9.48390454945879,-5.28011386077589));
#31797=CARTESIAN_POINT('Ctrl Pts',(23.3188386447889,-9.46702123153851,-5.25886285488616));
#31798=CARTESIAN_POINT('Ctrl Pts',(23.3227566922586,-9.44679191778429,-5.23340024926764));
#31799=CARTESIAN_POINT('Ctrl Pts',(23.3267923117017,-9.42796376054304,-5.20715758246077));
#31800=CARTESIAN_POINT('Ctrl Pts',(23.330940453435,-9.41048602013606,-5.18015433854917));
#31801=CARTESIAN_POINT('Ctrl Pts',(23.3351228528353,-9.39286393880524,-5.15292808679546));
#31802=CARTESIAN_POINT('Ctrl Pts',(23.3394201598385,-9.37661484871459,-5.12492704450796));
#31803=CARTESIAN_POINT('Ctrl Pts',(23.3438276432082,-9.36173991954695,-5.09617140010087));
#31804=CARTESIAN_POINT('Ctrl Pts',(23.3482277973286,-9.34688972605164,-5.06746357374989));
#31805=CARTESIAN_POINT('Ctrl Pts',(23.3527381839121,-9.3334098734431,-5.03800229552381));
#31806=CARTESIAN_POINT('Ctrl Pts',(23.3573474234541,-9.32134719718139,-5.00783018426007));
#31807=CARTESIAN_POINT('Ctrl Pts',(23.3594602261015,-9.31581785679728,-4.99399976473583));
#31808=CARTESIAN_POINT('Ctrl Pts',(23.36159366775,-9.31058685109039,-4.98002042570589));
#31809=CARTESIAN_POINT('Ctrl Pts',(23.3637458539898,-9.3056610997891,-4.9658989442033));
#31810=CARTESIAN_POINT('Ctrl Pts',(23.3689327974921,-9.2937896393951,-4.93186502772874));
#31811=CARTESIAN_POINT('Ctrl Pts',(23.3741744881082,-9.28381406376272,-4.89736287705005));
#31812=CARTESIAN_POINT('Ctrl Pts',(23.3794567597349,-9.27572244423294,-4.86250693594901));
#31813=CARTESIAN_POINT('Ctrl Pts',(23.3847141593254,-9.26766892479876,-4.82781511708374));
#31814=CARTESIAN_POINT('Ctrl Pts',(23.3900119424402,-9.261483515081,-4.79277205245652));
#31815=CARTESIAN_POINT('Ctrl Pts',(23.3953264024608,-9.25717549603294,-4.75753613869458));
#31816=CARTESIAN_POINT('Ctrl Pts',(23.4005606407812,-9.25293250647258,-4.72283211056155));
#31817=CARTESIAN_POINT('Ctrl Pts',(23.4058109474606,-9.25051245822955,-4.68794116925394));
#31818=CARTESIAN_POINT('Ctrl Pts',(23.4110447433103,-9.24991730685651,-4.65306327354699));
#31819=CARTESIAN_POINT('Ctrl Pts',(23.4118483764353,-9.24982592320849,-4.64770788080257));
#31820=CARTESIAN_POINT('Ctrl Pts',(23.4126516036639,-9.24977752137499,-4.64235288481083));
#31821=CARTESIAN_POINT('Ctrl Pts',(23.4134542901992,-9.24977205331206,-4.63699910361382));
#31822=CARTESIAN_POINT('Ctrl Pts',(32.4024604985347,-6.5271674865253,-5.07262713991703));
#31823=CARTESIAN_POINT('Ctrl Pts',(30.8491863429263,-5.4152335451132,-9.27174184877918));
#31824=CARTESIAN_POINT('Ctrl Pts',(30.8533045356553,-5.40952138499152,-4.65854638171772));
#31825=CARTESIAN_POINT('Ctrl Pts',(31.8738489475283,-7.26036572948979,-5.07124736770671));
#31826=CARTESIAN_POINT('Ctrl Pts',(30.4100357196107,-6.02337177536106,-9.27185079334058));
#31827=CARTESIAN_POINT('Ctrl Pts',(30.4152070763148,-6.01717418213576,-4.65727924423418));
#31828=CARTESIAN_POINT('Ctrl Pts',(31.2681650881339,-7.91543180451874,-5.06966586822249));
#31829=CARTESIAN_POINT('Ctrl Pts',(29.9069965319627,-6.56635458453651,-9.27197690985764));
#31830=CARTESIAN_POINT('Ctrl Pts',(29.9132343908402,-6.56007337164787,-4.65582684826234));
#31831=CARTESIAN_POINT('Ctrl Pts',(30.2492640515523,-8.7837432627388,-5.06700386436085));
#31832=CARTESIAN_POINT('Ctrl Pts',(29.061281076665,-7.28562977260592,-9.2721926629975));
#31833=CARTESIAN_POINT('Ctrl Pts',(29.0687996562966,-7.27970396316187,-4.65338215218851));
#31834=CARTESIAN_POINT('Ctrl Pts',(29.8894857961231,-9.05500734423673,-5.06606366510207));
#31835=CARTESIAN_POINT('Ctrl Pts',(28.7626222317253,-7.51031058116255,-9.27226941720439));
#31836=CARTESIAN_POINT('Ctrl Pts',(28.7706261881107,-7.50451952867758,-4.65251870436497));
#31837=CARTESIAN_POINT('Ctrl Pts',(29.1408971363909,-9.55118636769419,-5.06410680227813));
#31838=CARTESIAN_POINT('Ctrl Pts',(28.141312318348,-7.92115484476349,-9.27243052034795));
#31839=CARTESIAN_POINT('Ctrl Pts',(28.1502182742173,-7.91573787763376,-4.65072158676955));
#31840=CARTESIAN_POINT('Ctrl Pts',(28.7549938692441,-9.77457907404737,-5.06309774114963));
#31841=CARTESIAN_POINT('Ctrl Pts',(27.8210544714496,-8.10605040906689,-9.27251424317563));
#31842=CARTESIAN_POINT('Ctrl Pts',(27.830393176953,-8.10087907780255,-4.64979489842099));
#31843=CARTESIAN_POINT('Ctrl Pts',(27.9606791639968,-10.1734806965365,-5.06102010612066));
#31844=CARTESIAN_POINT('Ctrl Pts',(27.1619692903677,-8.43607716327051,-9.2726881271401));
#31845=CARTESIAN_POINT('Ctrl Pts',(27.1720888828609,-8.43147682347387,-4.64788686746487));
#31846=CARTESIAN_POINT('Ctrl Pts',(27.5522661850697,-10.3489863345078,-5.05995152857696));
#31847=CARTESIAN_POINT('Ctrl Pts',(26.8231243399103,-8.58119242091901,-9.27277829295598));
#31848=CARTESIAN_POINT('Ctrl Pts',(26.8336084090221,-8.57693065213295,-4.64690552139547));
#31849=CARTESIAN_POINT('Ctrl Pts',(26.7126541019217,-10.6515225006989,-5.05775402063874));
#31850=CARTESIAN_POINT('Ctrl Pts',(26.126651484303,-8.83118310305816,-9.27296539649543));
#31851=CARTESIAN_POINT('Ctrl Pts',(26.1377630016296,-8.82766358702302,-4.6448874029651));
#31852=CARTESIAN_POINT('Ctrl Pts',(26.2784387542335,-10.7790931636274,-5.05661718840921));
#31853=CARTESIAN_POINT('Ctrl Pts',(25.7665078239556,-8.93648699505751,-9.27306302841706));
#31854=CARTESIAN_POINT('Ctrl Pts',(25.7778982955421,-8.93339034065304,-4.64384337398737));
#31855=CARTESIAN_POINT('Ctrl Pts',(24.9693615852526,-11.0790942178393,-5.05318866423019));
#31856=CARTESIAN_POINT('Ctrl Pts',(24.6806743997377,-9.18386771107407,-9.27336026701782));
#31857=CARTESIAN_POINT('Ctrl Pts',(24.6929742515822,-9.18202225043396,-4.64069473154366));
#31858=CARTESIAN_POINT('Ctrl Pts',(24.0856759871579,-11.1726393389836,-5.05087270788765));
#31859=CARTESIAN_POINT('Ctrl Pts',(23.9480649578886,-9.26034679384409,-9.27356456879131));
#31860=CARTESIAN_POINT('Ctrl Pts',(23.9606020319037,-9.25954965162327,-4.63856783364609));
#31861=CARTESIAN_POINT('Ctrl Pts',(23.1912512483198,-11.1600029543462,-5.04852695082798));
#31862=CARTESIAN_POINT('Ctrl Pts',(23.2071698192741,-9.2489052015715,-9.27377520050524));
#31863=CARTESIAN_POINT('Ctrl Pts',(23.2193295343223,-9.24907699337613,-4.63641356863091));
#31864=CARTESIAN_POINT('Origin',(31.6603850692973,-6.,-4.65853571252147));
#31865=CARTESIAN_POINT('Origin',(31.6603850692973,-6.,-4.65853571252147));
#31866=CARTESIAN_POINT('Origin',(31.6603850692973,-6.,-4.65853571252147));
#31867=CARTESIAN_POINT('Origin',(23.3621596556826,-6.00000000000001,0.));
#31868=CARTESIAN_POINT('Origin',(-60.4312629272455,-6.00000000000007,-3.60555127546388));
#31869=CARTESIAN_POINT('Origin',(31.6603850692973,-6.00000000000007,-3.60555127546388));
#31870=CARTESIAN_POINT('Origin',(31.6603850692973,-6.,-3.60555127546399));
#31871=CARTESIAN_POINT('Origin',(31.6603850692973,-6.,-3.60555127546399));
#31872=CARTESIAN_POINT('Ctrl Pts',(30.8540107833128,-5.40854159976692,-3.61676245694848));
#31873=CARTESIAN_POINT('Ctrl Pts',(31.1246510147285,-5.03304526370463,-3.27244402074537));
#31874=CARTESIAN_POINT('Ctrl Pts',(31.6652680269928,-5.13707314618097,-3.10007755425091));
#31875=CARTESIAN_POINT('Ctrl Pts',(30.7245581660947,-5.58814855488697,-3.28694957845087));
#31876=CARTESIAN_POINT('Ctrl Pts',(31.0038498616761,-5.2193924464231,-2.98485241905846));
#31877=CARTESIAN_POINT('Ctrl Pts',(31.521826137082,-5.3076575752865,-2.81739272721273));
#31878=CARTESIAN_POINT('Ctrl Pts',(30.6026936291093,-5.74365115677863,-2.94054961542029));
#31879=CARTESIAN_POINT('Ctrl Pts',(30.8866588414047,-5.38513818005051,-2.67536548262944));
#31880=CARTESIAN_POINT('Ctrl Pts',(31.3867827859884,-5.45535959933227,-2.52047224429094));
#31881=CARTESIAN_POINT('Ctrl Pts',(30.4952922544521,-5.87429133955086,-2.57456137432713));
#31882=CARTESIAN_POINT('Ctrl Pts',(30.7821008780688,-5.52542682927969,-2.343319664422));
#31883=CARTESIAN_POINT('Ctrl Pts',(31.2677682718374,-5.57944414885907,-2.206763327537));
#31884=CARTESIAN_POINT('Origin',(31.2718056654608,-6.50442118859734,-2.5869876306867));
#31885=CARTESIAN_POINT('Ctrl Pts',(30.5324890548671,-5.82879633920879,-2.71722364618277));
#31886=CARTESIAN_POINT('Ctrl Pts',(30.8338107320096,-5.45071871851039,-2.46481580902341));
#31887=CARTESIAN_POINT('Ctrl Pts',(31.3550349630983,-5.53239849610685,-2.3266043417601));
#31888=CARTESIAN_POINT('Ctrl Pts',(30.414072865639,-5.97470345390586,-2.316286616319));
#31889=CARTESIAN_POINT('Ctrl Pts',(30.6750363657221,-5.66357496609264,-2.13638111093782));
#31890=CARTESIAN_POINT('Ctrl Pts',(31.0916380800151,-5.66597009492328,-1.98109641144098));
#31891=CARTESIAN_POINT('Ctrl Pts',(30.2983091365626,-6.10823981714543,-1.91022886595462));
#31892=CARTESIAN_POINT('Ctrl Pts',(30.5109747166508,-5.86560552736745,-1.77125969601649));
#31893=CARTESIAN_POINT('Ctrl Pts',(30.8338791248953,-5.81481785500372,-1.64351567473586));
#31894=CARTESIAN_POINT('Ctrl Pts',(30.1385677084671,-6.28357646880036,-1.3132741814918));
#31895=CARTESIAN_POINT('Ctrl Pts',(30.2801036148756,-6.12983921074557,-1.22538124018223));
#31896=CARTESIAN_POINT('Ctrl Pts',(30.4777418384395,-6.05616287591927,-1.14217293852664));
#31897=CARTESIAN_POINT('Ctrl Pts',(30.0904315385969,-6.33514385852499,-1.12739899919828));
#31898=CARTESIAN_POINT('Ctrl Pts',(30.2102025602331,-6.20727944608654,-1.05512647412131));
#31899=CARTESIAN_POINT('Ctrl Pts',(30.3703800811856,-6.1339441904561,-0.985420405775108));
#31900=CARTESIAN_POINT('Ctrl Pts',(30.018023994589,-6.41102310169597,-0.848150890259438));
#31901=CARTESIAN_POINT('Ctrl Pts',(30.1026491762848,-6.32269295519541,-0.797099276114036));
#31902=CARTESIAN_POINT('Ctrl Pts',(30.2087777149437,-6.26088647609721,-0.747200281085206));
#31903=CARTESIAN_POINT('Ctrl Pts',(29.9939866367595,-6.43594024923508,-0.754898211424712));
#31904=CARTESIAN_POINT('Ctrl Pts',(30.0666264056926,-6.36077277190929,-0.710692186109099));
#31905=CARTESIAN_POINT('Ctrl Pts',(30.1551143502848,-6.30461258601909,-0.667187369252594));
#31906=CARTESIAN_POINT('Ctrl Pts',(29.9553790818645,-6.47547849065892,-0.616730145059731));
#31907=CARTESIAN_POINT('Ctrl Pts',(30.0077313439108,-6.42194755412475,-0.582137175444621));
#31908=CARTESIAN_POINT('Ctrl Pts',(30.0688833690653,-6.37844917842461,-0.547904805602633));
#31909=CARTESIAN_POINT('Ctrl Pts',(29.9421730778576,-6.48893120155848,-0.570837627283043));
#31910=CARTESIAN_POINT('Ctrl Pts',(29.9874546393352,-6.44285275085176,-0.539374301820755));
#31911=CARTESIAN_POINT('Ctrl Pts',(30.0393820383596,-6.40423350461356,-0.508152377116182));
#31912=CARTESIAN_POINT('Ctrl Pts',(29.9194851596862,-6.51187275945457,-0.504345210892826));
#31913=CARTESIAN_POINT('Ctrl Pts',(29.9521600875081,-6.47885302842194,-0.477362421809093));
#31914=CARTESIAN_POINT('Ctrl Pts',(29.9886822113593,-6.45001927031411,-0.45051366532455));
#31915=CARTESIAN_POINT('Ctrl Pts',(29.9114793064789,-6.51994455052701,-0.482456574337637));
#31916=CARTESIAN_POINT('Ctrl Pts',(29.9396491544529,-6.4915613908261,-0.456942353896258));
#31917=CARTESIAN_POINT('Ctrl Pts',(29.9707897557899,-6.46637912941077,-0.431525520814346));
#31918=CARTESIAN_POINT('Ctrl Pts',(29.8743743869234,-6.55717647646013,-0.404137800076886));
#31919=CARTESIAN_POINT('Ctrl Pts',(29.8811504343294,-6.55057084913525,-0.384098298935905));
#31920=CARTESIAN_POINT('Ctrl Pts',(29.8878444644056,-6.54394119315548,-0.363954837557253));
#31921=CARTESIAN_POINT('Ctrl Pts',(29.8326596614655,-6.59883470986062,-0.326319010490884));
#31922=CARTESIAN_POINT('Ctrl Pts',(29.8141830203482,-6.61768161165595,-0.311268651041244));
#31923=CARTESIAN_POINT('Ctrl Pts',(29.7933669799477,-6.63390835381247,-0.296165474079821));
#31924=CARTESIAN_POINT('Ctrl Pts',(29.6859854969601,-6.74216993980689,-0.814345382263683));
#31925=CARTESIAN_POINT('Ctrl Pts',(29.5721084772451,-6.8527104879045,-0.782222273536295));
#31926=CARTESIAN_POINT('Ctrl Pts',(29.4730487580193,-6.97593588682555,-0.747368780897885));
#31927=CARTESIAN_POINT('Origin',(30.5687260201471,-7.27684647674051,-0.418815697553272));
#31928=CARTESIAN_POINT('Ctrl Pts',(29.8644600669621,-6.56691023510729,-0.418815697553251));
#31929=CARTESIAN_POINT('Ctrl Pts',(29.8672867891358,-6.56410609007334,-0.22564283964309));
#31930=CARTESIAN_POINT('Ctrl Pts',(29.9206004593126,-6.61260230756601,-0.0463738348445692));
#31931=CARTESIAN_POINT('Ctrl Pts',(29.4322533561227,-6.99566489409189,-0.404910666486995));
#31932=CARTESIAN_POINT('Ctrl Pts',(29.4355057872863,-6.99280750543929,-0.218180296639813));
#31933=CARTESIAN_POINT('Ctrl Pts',(29.481561161048,-7.04232459329972,-0.0439899824717745));
#31934=CARTESIAN_POINT('Ctrl Pts',(28.9652970371703,-7.37504694162997,-0.389236972868619));
#31935=CARTESIAN_POINT('Ctrl Pts',(28.9689298214357,-7.37227200661717,-0.209763874461039));
#31936=CARTESIAN_POINT('Ctrl Pts',(29.0084787340067,-7.42047716376697,-0.0414223856508554));
#31937=CARTESIAN_POINT('Ctrl Pts',(28.2150317307457,-7.8729956694109,-0.361993861939527));
#31938=CARTESIAN_POINT('Ctrl Pts',(28.2191095777036,-7.87047110758279,-0.195122273103594));
#31939=CARTESIAN_POINT('Ctrl Pts',(28.2510459088753,-7.91449073927164,-0.037280815250846));
#31940=CARTESIAN_POINT('Ctrl Pts',(27.956570399131,-8.02704348376974,-0.352282263845473));
#31941=CARTESIAN_POINT('Ctrl Pts',(27.9608114812428,-8.02460729347139,-0.189901771615212));
#31942=CARTESIAN_POINT('Ctrl Pts',(27.9899390476894,-8.06714077884413,-0.0358480736072952));
#31943=CARTESIAN_POINT('Ctrl Pts',(27.422538725282,-8.31073680629816,-0.331227233487651));
#31944=CARTESIAN_POINT('Ctrl Pts',(27.4270826096138,-8.30850613456263,-0.178579183139945));
#31945=CARTESIAN_POINT('Ctrl Pts',(27.4509872039948,-8.34755545461492,-0.0328670883961612));
#31946=CARTESIAN_POINT('Ctrl Pts',(27.1459961653714,-8.44062057060663,-0.319840425202939));
#31947=CARTESIAN_POINT('Ctrl Pts',(27.15068459432,-8.43851047177455,-0.172453929810078));
#31948=CARTESIAN_POINT('Ctrl Pts',(27.1720884374499,-8.47550022999066,-0.0313130112254784));
#31949=CARTESIAN_POINT('Ctrl Pts',(26.3082189750106,-8.78499234568452,-0.28314310589906));
#31950=CARTESIAN_POINT('Ctrl Pts',(26.3133627198456,-8.7832436968066,-0.152707180606665));
#31951=CARTESIAN_POINT('Ctrl Pts',(26.3268414702778,-8.81402640047916,-0.0265301127609303));
#31952=CARTESIAN_POINT('Ctrl Pts',(25.7337629486952,-8.95777986606701,-0.255738121841735));
#31953=CARTESIAN_POINT('Ctrl Pts',(25.7391198628699,-8.95635681278008,-0.137952410902559));
#31954=CARTESIAN_POINT('Ctrl Pts',(25.7488742137392,-8.98148038394029,-0.0232071389870805));
#31955=CARTESIAN_POINT('Ctrl Pts',(24.8488322354996,-9.13271117527261,-0.201422710338595));
#31956=CARTESIAN_POINT('Ctrl Pts',(24.85431631276,-9.13180909992311,-0.108676967321741));
#31957=CARTESIAN_POINT('Ctrl Pts',(24.8618592937854,-9.14780634343858,-0.0174743900899742));
#31958=CARTESIAN_POINT('Ctrl Pts',(24.5493473176432,-9.17693685209723,-0.181278555574678));
#31959=CARTESIAN_POINT('Ctrl Pts',(24.5548852729846,-9.17621341858475,-0.0978176119286749));
#31960=CARTESIAN_POINT('Ctrl Pts',(24.5614827959266,-9.18906214293745,-0.0154452600370327));
#31961=CARTESIAN_POINT('Ctrl Pts',(24.0962646566309,-9.22109619601667,-0.141898246278996));
#31962=CARTESIAN_POINT('Ctrl Pts',(24.1018342618134,-9.22064518679162,-0.0765766260304406));
#31963=CARTESIAN_POINT('Ctrl Pts',(24.1078835619629,-9.22867390569795,-0.0117975702348942));
#31964=CARTESIAN_POINT('Ctrl Pts',(23.9451103869883,-9.23207461097023,-0.127435185337285));
#31965=CARTESIAN_POINT('Ctrl Pts',(23.9506929727475,-9.23171479242211,-0.0687748081469021));
#31966=CARTESIAN_POINT('Ctrl Pts',(23.9565156706971,-9.23812508071924,-0.0104948818754195));
#31967=CARTESIAN_POINT('Ctrl Pts',(23.7185889926574,-9.24296254743562,-0.0993609997538649));
#31968=CARTESIAN_POINT('Ctrl Pts',(23.7241791415465,-9.24273959271718,-0.0536265938788905));
#31969=CARTESIAN_POINT('Ctrl Pts',(23.7298736629463,-9.24671619801047,-0.00808004655455183));
#31970=CARTESIAN_POINT('Ctrl Pts',(23.6430586656737,-9.2456625586093,-0.089045290078164));
#31971=CARTESIAN_POINT('Ctrl Pts',(23.6486519255516,-9.24548527128067,-0.0480602081809084));
#31972=CARTESIAN_POINT('Ctrl Pts',(23.6542931292373,-9.24864855291419,-0.00720601563352635));
#31973=CARTESIAN_POINT('Ctrl Pts',(23.5302452018234,-9.24832020150248,-0.0689516266792481));
#31974=CARTESIAN_POINT('Ctrl Pts',(23.5358401824189,-9.24821115604552,-0.0372161319416783));
#31975=CARTESIAN_POINT('Ctrl Pts',(23.5414539113024,-9.25015795747161,-0.00554437323078288));
#31976=CARTESIAN_POINT('Ctrl Pts',(23.4927698292594,-9.24897232310166,-0.0615775233974875));
#31977=CARTESIAN_POINT('Ctrl Pts',(23.4983655159144,-9.24888594108447,-0.0332364108970037));
#31978=CARTESIAN_POINT('Ctrl Pts',(23.5039677092379,-9.25042838173558,-0.00493933046707393));
#31979=CARTESIAN_POINT('Ctrl Pts',(23.437207464985,-9.24960744693864,-0.047173048025456));
#31980=CARTESIAN_POINT('Ctrl Pts',(23.4428035048708,-9.24955468884453,-0.025461954196264));
#31981=CARTESIAN_POINT('Ctrl Pts',(23.4484009772938,-9.25049704610979,-0.00377193262624975));
#31982=CARTESIAN_POINT('Ctrl Pts',(23.4187809144,-9.2497619746319,-0.0418867767987868));
#31983=CARTESIAN_POINT('Ctrl Pts',(23.4243771019783,-9.24972035740697,-0.022608789399977));
#31984=CARTESIAN_POINT('Ctrl Pts',(23.4299724616912,-9.25046369517988,-0.00334517687545925));
#31985=CARTESIAN_POINT('Ctrl Pts',(23.391639961472,-9.24991070032528,-0.0314080342235584));
#31986=CARTESIAN_POINT('Ctrl Pts',(23.3972362039634,-9.24988551015033,-0.0169528988061137));
#31987=CARTESIAN_POINT('Ctrl Pts',(23.4028313580097,-9.250335588764,-0.00250444453845097));
#31988=CARTESIAN_POINT('Ctrl Pts',(23.3826392408352,-9.24994623900697,-0.0275171890118582));
#31989=CARTESIAN_POINT('Ctrl Pts',(23.3882355060456,-9.24992647330526,-0.0148528068526551));
#31990=CARTESIAN_POINT('Ctrl Pts',(23.3938305105107,-9.25027946927614,-0.00219288882915726));
#31991=CARTESIAN_POINT('Ctrl Pts',(23.3658173417907,-9.2499903003333,-0.0174297620612975));
#31992=CARTESIAN_POINT('Ctrl Pts',(23.3714136289275,-9.24998074934077,-0.00940802009743088));
#31993=CARTESIAN_POINT('Ctrl Pts',(23.377008722703,-9.25015155434988,-0.00138747258816392));
#31994=CARTESIAN_POINT('Ctrl Pts',(23.3554916517933,-9.2499983698261,-0.011326547126086));
#31995=CARTESIAN_POINT('Ctrl Pts',(23.3610879101787,-9.24999839768389,-0.00611426124958945));
#31996=CARTESIAN_POINT('Ctrl Pts',(23.3666837799662,-9.24999842553965,-0.000902536247986865));
#31997=CARTESIAN_POINT('Ctrl Pts',(23.3560798278474,-9.24999837277875,2.22339565558631E-11));
#31998=CARTESIAN_POINT('Ctrl Pts',(23.3560798278474,-9.24999837277876,2.22339565558632E-11));
#31999=CARTESIAN_POINT('Ctrl Pts',(23.3560798278469,-9.24999837277874,2.22339565558627E-11));
#32000=CARTESIAN_POINT('',(0.,0.,0.));
#32001=CARTESIAN_POINT('Origin',(0.,0.,0.));
#32002=CARTESIAN_POINT('',(-1.36919674566051E-15,-11.1803398874989,-10.));
#32003=CARTESIAN_POINT('',(-1.36919674566051E-15,-11.1803398874989,10.));
#32004=CARTESIAN_POINT('Origin',(0.,0.,0.));
#32005=CARTESIAN_POINT('',(11.1803398874989,0.,-10.));
#32006=CARTESIAN_POINT('Origin',(0.,0.,-10.));
#32007=CARTESIAN_POINT('',(11.1803398874989,0.,10.));
#32008=CARTESIAN_POINT('Origin',(11.1803398874989,0.,0.));
#32009=CARTESIAN_POINT('Origin',(0.,0.,10.));
#32010=CARTESIAN_POINT('Origin',(0.,0.,-10.));
#32011=CARTESIAN_POINT('',(-6.,-7.34788079488412E-16,-10.));
#32012=CARTESIAN_POINT('Origin',(0.,0.,-10.));
#32013=CARTESIAN_POINT('',(-6.,-7.34788079488412E-16,10.));
#32014=CARTESIAN_POINT('',(-6.,-7.34788079488412E-16,-10.));
#32015=CARTESIAN_POINT('Origin',(0.,0.,10.));
#32016=CARTESIAN_POINT('Origin',(0.,0.,0.));
#32017=CARTESIAN_POINT('Origin',(0.,0.,10.));
#32018=CARTESIAN_POINT('Origin',(11.1803398874989,0.,0.));
#32019=CARTESIAN_POINT('Origin',(0.,0.,-10.));
#32020=CARTESIAN_POINT('Origin',(130.,0.,0.));
#32021=CARTESIAN_POINT('',(130.,-7.34788079488412E-16,-6.));
#32022=CARTESIAN_POINT('',(130.,-7.34788079488412E-16,-6.));
#32023=CARTESIAN_POINT('Origin',(130.,0.,0.));
#32024=CARTESIAN_POINT('Origin',(-71.1905382258649,0.,0.));
#32025=CARTESIAN_POINT('',(149.5,-7.34788079488412E-16,-6.));
#32026=CARTESIAN_POINT('',(-71.1905382258649,-7.34788079488412E-16,-6.));
#32027=CARTESIAN_POINT('Origin',(149.5,0.,0.));
#32028=CARTESIAN_POINT('Origin',(150.,0.,0.));
#32029=CARTESIAN_POINT('',(150.,-6.73555739531044E-16,-5.5));
#32030=CARTESIAN_POINT('',(150.,-6.73555739531044E-16,-5.5));
#32031=CARTESIAN_POINT('Origin',(150.,0.,0.));
#32032=CARTESIAN_POINT('Origin',(150.,0.,0.));
#32033=CARTESIAN_POINT('Origin',(11.1803398874989,-15.,10.));
#32034=CARTESIAN_POINT('Origin',(11.1803398874989,-15.,-10.));
#32035=CARTESIAN_POINT('',(0.,0.,0.));
#32036=CARTESIAN_POINT('Origin',(14.8870768733179,-3.99420842564088,0.));
#32037=CARTESIAN_POINT('',(18.3575990203927,-3.99420842564088,4.26678755349543));
#32038=CARTESIAN_POINT('',(11.5587496781628,-3.99420842549338,4.37861311631065));
#32039=CARTESIAN_POINT('Origin',(14.8870768733179,-3.99420842564088,0.));
#32040=CARTESIAN_POINT('',(18.3843475112712,-4.12317055822481,4.26678755349543));
#32041=CARTESIAN_POINT('Ctrl Pts',(18.3843475112712,-4.1231705582248,4.26678755349543));
#32042=CARTESIAN_POINT('Ctrl Pts',(18.3672627745756,-4.08260100655593,4.26678755349543));
#32043=CARTESIAN_POINT('Ctrl Pts',(18.3575990203927,-4.03574406331344,4.26678755349543));
#32044=CARTESIAN_POINT('Ctrl Pts',(18.3575990203927,-3.99420842564088,4.26678755349543));
#32045=CARTESIAN_POINT('',(18.7837086993174,-4.27128032554705,5.09745204146194));
#32046=CARTESIAN_POINT('Ctrl Pts',(18.7837086993174,-4.27128032554705,5.09745204146194));
#32047=CARTESIAN_POINT('Ctrl Pts',(18.7837837490088,-4.27218840717948,5.09663376751006));
#32048=CARTESIAN_POINT('Ctrl Pts',(18.7838568749948,-4.27309451506193,5.09581312836018));
#32049=CARTESIAN_POINT('Ctrl Pts',(18.786376054168,-4.30508335769532,5.0666946999686));
#32050=CARTESIAN_POINT('Ctrl Pts',(18.7865447928184,-4.33378349175756,5.03565092415356));
#32051=CARTESIAN_POINT('Ctrl Pts',(18.7822885734857,-4.38502690350443,4.96945449120915));
#32052=CARTESIAN_POINT('Ctrl Pts',(18.7779104286292,-4.40756216172138,4.93442106198759));
#32053=CARTESIAN_POINT('Ctrl Pts',(18.7601365382803,-4.4586258081985,4.8363053847714));
#32054=CARTESIAN_POINT('Ctrl Pts',(18.7426983881329,-4.48040963095378,4.77095332236947));
#32055=CARTESIAN_POINT('Ctrl Pts',(18.6987452289246,-4.49763058563495,4.64635114121833));
#32056=CARTESIAN_POINT('Ctrl Pts',(18.6736500581964,-4.49538158540805,4.58805456925361));
#32057=CARTESIAN_POINT('Ctrl Pts',(18.6187727586818,-4.46886694818906,4.48266333773381));
#32058=CARTESIAN_POINT('Ctrl Pts',(18.5900193347752,-4.44634242811073,4.43625626352526));
#32059=CARTESIAN_POINT('Ctrl Pts',(18.5302580379935,-4.38241110798174,4.35685111603697));
#32060=CARTESIAN_POINT('Ctrl Pts',(18.500152649712,-4.34177888816883,4.32523467597912));
#32061=CARTESIAN_POINT('Ctrl Pts',(18.4403522870749,-4.24412140399772,4.27947358970446));
#32062=CARTESIAN_POINT('Ctrl Pts',(18.4118332395335,-4.18772090860718,4.26754505508647));
#32063=CARTESIAN_POINT('Ctrl Pts',(18.3859538609649,-4.12697400251701,4.26679918369438));
#32064=CARTESIAN_POINT('Ctrl Pts',(18.3851486227203,-4.12507288384488,4.26678755349543));
#32065=CARTESIAN_POINT('Ctrl Pts',(18.3843475112712,-4.1231705582248,4.26678755349543));
#32066=CARTESIAN_POINT('',(14.8870768733179,-4.27128032554705,6.41621047834285));
#32067=CARTESIAN_POINT('Origin',(14.8870768733179,-4.27128032554705,0.));
#32068=CARTESIAN_POINT('',(11.1121596556826,-4.27128032554705,5.18823254127999));
#32069=CARTESIAN_POINT('Origin',(14.8870768733179,-4.27128032554705,0.));
#32070=CARTESIAN_POINT('',(11.1585526808199,-4.38134327817891,5.09856534363104));
#32071=CARTESIAN_POINT('Ctrl Pts',(11.1585526808199,-4.3813432781789,5.09856534363105));
#32072=CARTESIAN_POINT('Ctrl Pts',(11.1473312438077,-4.36992324654723,5.10766848669372));
#32073=CARTESIAN_POINT('Ctrl Pts',(11.1380491180006,-4.35765259554692,5.11756292166355));
#32074=CARTESIAN_POINT('Ctrl Pts',(11.1191192706006,-4.32341816221833,5.14537473079008));
#32075=CARTESIAN_POINT('Ctrl Pts',(11.1134224194163,-4.30138253065776,5.163462535227));
#32076=CARTESIAN_POINT('Ctrl Pts',(11.1122215415905,-4.27651763887363,5.18392138130289));
#32077=CARTESIAN_POINT('Ctrl Pts',(11.1121596556826,-4.27389704286368,5.18607829451038));
#32078=CARTESIAN_POINT('Ctrl Pts',(11.1121596556826,-4.27128032554705,5.18823254127999));
#32079=CARTESIAN_POINT('Ctrl Pts',(11.1585526808199,-4.3813432781789,5.09856534363102));
#32080=CARTESIAN_POINT('Ctrl Pts',(11.1773095549183,-4.40043210755625,5.08334924344489));
#32081=CARTESIAN_POINT('Ctrl Pts',(11.1965634151784,-4.4173731502363,5.06638959987712));
#32082=CARTESIAN_POINT('Ctrl Pts',(11.2160327365605,-4.43193019076584,5.04794583007894));
#32083=CARTESIAN_POINT('Ctrl Pts',(11.2354990641271,-4.44648499284589,5.02950489639618));
#32084=CARTESIAN_POINT('Ctrl Pts',(11.2551808642034,-4.45865655252623,5.00958029965859));
#32085=CARTESIAN_POINT('Ctrl Pts',(11.274792429352,-4.46825273239085,4.9884587446323));
#32086=CARTESIAN_POINT('Ctrl Pts',(11.2941553532197,-4.47772724902083,4.96760497498952));
#32087=CARTESIAN_POINT('Ctrl Pts',(11.3134499546024,-4.48469120840074,4.94558444999912));
#32088=CARTESIAN_POINT('Ctrl Pts',(11.3323953871065,-4.4890027089001,4.92269940887843));
#32089=CARTESIAN_POINT('Ctrl Pts',(11.3351876324295,-4.48963815320058,4.91932653000516));
#32090=CARTESIAN_POINT('Ctrl Pts',(11.337972280205,-4.49021605981353,4.91593491859636));
#32091=CARTESIAN_POINT('Ctrl Pts',(11.3407484170913,-4.49073605743567,4.91252559036269));
#32092=CARTESIAN_POINT('Ctrl Pts',(11.3547633161211,-4.49336118525475,4.89531412244499));
#32093=CARTESIAN_POINT('Ctrl Pts',(11.3685552099561,-4.49450846568624,4.87762256908791));
#32094=CARTESIAN_POINT('Ctrl Pts',(11.3819878602125,-4.49414152262893,4.85965719763341));
#32095=CARTESIAN_POINT('Ctrl Pts',(11.395405640951,-4.49377498576595,4.84171171327548));
#32096=CARTESIAN_POINT('Ctrl Pts',(11.408464565942,-4.49189752730246,4.82349370723299));
#32097=CARTESIAN_POINT('Ctrl Pts',(11.4210277728039,-4.4885248109505,4.80521097378518));
#32098=CARTESIAN_POINT('Ctrl Pts',(11.4335822281363,-4.48515444403263,4.78694097608885));
#32099=CARTESIAN_POINT('Ctrl Pts',(11.4456412560887,-4.4802910478885,4.76860702043866));
#32100=CARTESIAN_POINT('Ctrl Pts',(11.4570732740609,-4.47400139883477,4.75040836654866));
#32101=CARTESIAN_POINT('Ctrl Pts',(11.4685151056053,-4.46770635056582,4.73219409041199));
#32102=CARTESIAN_POINT('Ctrl Pts',(11.4793284781842,-4.45998292162542,4.71411597746148));
#32103=CARTESIAN_POINT('Ctrl Pts',(11.4893922899608,-4.45094580241425,4.69635581925144));
#32104=CARTESIAN_POINT('Ctrl Pts',(11.4920989042063,-4.4485153122443,4.69157930928875));
#32105=CARTESIAN_POINT('Ctrl Pts',(11.4947513791458,-4.44599005094235,4.68682566810614));
#32106=CARTESIAN_POINT('Ctrl Pts',(11.4973475437826,-4.44337278307003,4.68209812382832));
#32107=CARTESIAN_POINT('Ctrl Pts',(11.5077296350369,-4.43290629974226,4.66319262168678));
#32108=CARTESIAN_POINT('Ctrl Pts',(11.5172734125896,-4.42090574709578,4.6446023839419));
#32109=CARTESIAN_POINT('Ctrl Pts',(11.5258955869574,-4.40751314754861,4.62655201641239));
#32110=CARTESIAN_POINT('Ctrl Pts',(11.5345249584578,-4.3941093688822,4.60848658181469));
#32111=CARTESIAN_POINT('Ctrl Pts',(11.5422308699739,-4.37931167764824,4.5909623828728));
#32112=CARTESIAN_POINT('Ctrl Pts',(11.5489433162914,-4.36330323603289,4.57417465116161));
#32113=CARTESIAN_POINT('Ctrl Pts',(11.5556857006915,-4.34722339540369,4.55731204473634));
#32114=CARTESIAN_POINT('Ctrl Pts',(11.5614254453185,-4.32992254541911,4.54119286157319));
#32115=CARTESIAN_POINT('Ctrl Pts',(11.5661098411332,-4.31161973967048,4.52597841654563));
#32116=CARTESIAN_POINT('Ctrl Pts',(11.5705971850955,-4.29408685216071,4.51140397605518));
#32117=CARTESIAN_POINT('Ctrl Pts',(11.5741160472691,-4.27563526415159,4.49765968025081));
#32118=CARTESIAN_POINT('Ctrl Pts',(11.5766390463652,-4.25647826147709,4.48485227018126));
#32119=CARTESIAN_POINT('Ctrl Pts',(11.5794931650578,-4.23480708469628,4.47036400954688));
#32120=CARTESIAN_POINT('Ctrl Pts',(11.5810960704826,-4.21214692060508,4.4570253967079));
#32121=CARTESIAN_POINT('Ctrl Pts',(11.5814513272692,-4.18878092059738,4.44498843498031));
#32122=CARTESIAN_POINT('Ctrl Pts',(11.5818079107915,-4.1653276583371,4.43290652022721));
#32123=CARTESIAN_POINT('Ctrl Pts',(11.5809072718065,-4.14116392290607,4.42213601639323));
#32124=CARTESIAN_POINT('Ctrl Pts',(11.5787776008328,-4.1165901294392,4.41278615288452));
#32125=CARTESIAN_POINT('Ctrl Pts',(11.5766350579062,-4.09186780940795,4.40337977782801));
#32126=CARTESIAN_POINT('Ctrl Pts',(11.5732483837397,-4.06673113295231,4.39541118325963));
#32127=CARTESIAN_POINT('Ctrl Pts',(11.568674438697,-4.04149025084392,4.38894711814017));
#32128=CARTESIAN_POINT('Ctrl Pts',(11.5658212792949,-4.02574536116308,4.38491492973413));
#32129=CARTESIAN_POINT('Ctrl Pts',(11.5625067173604,-4.00995996944461,4.38146728159866));
#32130=CARTESIAN_POINT('Ctrl Pts',(11.5587504889214,-3.99420842564088,4.37861204937474));
#32131=CARTESIAN_POINT('Origin',(14.8870768733179,-10.,0.));
#32132=CARTESIAN_POINT('',(11.5587511938191,-3.99420842554644,-4.37861112231563));
#32133=CARTESIAN_POINT('',(18.3575990203927,-3.99420842564088,-4.26678755349543));
#32134=CARTESIAN_POINT('Origin',(14.8870768733179,-3.99420842564088,0.));
#32135=CARTESIAN_POINT('',(18.3575990203927,0.,-4.26678755349543));
#32136=CARTESIAN_POINT('',(18.3575990203927,-10.,-4.26678755349543));
#32137=CARTESIAN_POINT('',(11.1121596556826,0.,-4.));
#32138=CARTESIAN_POINT('Origin',(14.8870768733179,0.,0.));
#32139=CARTESIAN_POINT('',(11.1121596556826,0.,4.));
#32140=CARTESIAN_POINT('Ctrl Pts',(11.1121596556826,-1.38777878078145E-16,
4.));
#32141=CARTESIAN_POINT('Ctrl Pts',(11.1121596556826,-0.533653252111662,
4.));
#32142=CARTESIAN_POINT('Ctrl Pts',(10.9882952072323,-1.0734712657027,3.88925687843601));
#32143=CARTESIAN_POINT('Ctrl Pts',(10.6170666685974,-2.04568897841338,3.47761758578428));
#32144=CARTESIAN_POINT('Ctrl Pts',(10.3784032063556,-2.48101536396881,3.17583888552357));
#32145=CARTESIAN_POINT('Ctrl Pts',(9.96544313722852,-3.16971217824285,2.48714207124953));
#32146=CARTESIAN_POINT('Ctrl Pts',(9.75819541135692,-3.47527655703118,2.0509015186475));
#32147=CARTESIAN_POINT('Ctrl Pts',(9.46796099283537,-3.89087901668554,1.06995606602431));
#32148=CARTESIAN_POINT('Ctrl Pts',(9.38707687331794,-4.,0.524242122051539));
#32149=CARTESIAN_POINT('Ctrl Pts',(9.38707687331794,-4.,-0.524242122051539));
#32150=CARTESIAN_POINT('Ctrl Pts',(9.46796099283537,-3.89087901668554,-1.06995606602431));
#32151=CARTESIAN_POINT('Ctrl Pts',(9.75819541135692,-3.47527655703118,-2.0509015186475));
#32152=CARTESIAN_POINT('Ctrl Pts',(9.96544313722852,-3.16971217824285,-2.48714207124953));
#32153=CARTESIAN_POINT('Ctrl Pts',(10.3784032063556,-2.48101536396881,-3.17583888552357));
#32154=CARTESIAN_POINT('Ctrl Pts',(10.6170666685974,-2.04568897841338,-3.47761758578428));
#32155=CARTESIAN_POINT('Ctrl Pts',(10.9882952072323,-1.0734712657027,-3.88925687843601));
#32156=CARTESIAN_POINT('Ctrl Pts',(11.1121596556826,-0.533653252111662,
-4.));
#32157=CARTESIAN_POINT('Ctrl Pts',(11.1121596556826,3.46944695195361E-17,
-4.));
#32158=CARTESIAN_POINT('',(18.3575990203927,0.,4.26678755349543));
#32159=CARTESIAN_POINT('Origin',(14.8870768733179,0.,0.));
#32160=CARTESIAN_POINT('',(18.3575990203927,-10.,4.26678755349543));
#32161=CARTESIAN_POINT('Ctrl Pts',(11.5587480564523,-3.99420842537537,4.37861525003541));
#32162=CARTESIAN_POINT('Ctrl Pts',(11.3626888290799,-4.17260831802453,4.2296270579284));
#32163=CARTESIAN_POINT('Ctrl Pts',(11.1762509051612,-4.34724444370875,4.06742136026345));
#32164=CARTESIAN_POINT('Ctrl Pts',(10.9996449425516,-4.51555528763266,3.89087737077926));
#32165=CARTESIAN_POINT('Ctrl Pts',(10.9109832717729,-4.60005255155271,3.80224681243159));
#32166=CARTESIAN_POINT('Ctrl Pts',(10.8247992487372,-4.68295483008131,3.71000257036262));
#32167=CARTESIAN_POINT('Ctrl Pts',(10.7411172332764,-4.76393373085428,3.61400313546724));
#32168=CARTESIAN_POINT('Ctrl Pts',(10.7349938888345,-4.76985927769047,3.60697847666982));
#32169=CARTESIAN_POINT('Ctrl Pts',(10.7288840068187,-4.77577479692699,3.5999334249579));
#32170=CARTESIAN_POINT('Ctrl Pts',(10.7227876488657,-4.7816801689495,3.5928678430334));
#32171=CARTESIAN_POINT('Ctrl Pts',(10.5986546413389,-4.90192435332469,3.44899966124763));
#32172=CARTESIAN_POINT('Ctrl Pts',(10.4800584128371,-5.01802447019821,3.29654164157823));
#32173=CARTESIAN_POINT('Ctrl Pts',(10.3675209931788,-5.12895882939301,3.13426461014042));
#32174=CARTESIAN_POINT('Ctrl Pts',(10.3643044716539,-5.13212953257135,3.12962644119902));
#32175=CARTESIAN_POINT('Ctrl Pts',(10.3610927721511,-5.13529615364872,3.12497977289136));
#32176=CARTESIAN_POINT('Ctrl Pts',(10.357885971712,-5.13845860697225,3.12032468109803));
#32177=CARTESIAN_POINT('Ctrl Pts',(10.2726922148679,-5.222474212119,2.99665475967357));
#32178=CARTESIAN_POINT('Ctrl Pts',(10.1909180066101,-5.30357974676513,2.86698461435898));
#32179=CARTESIAN_POINT('Ctrl Pts',(10.1140426590526,-5.38013901643824,2.73275773423716));
#32180=CARTESIAN_POINT('Ctrl Pts',(10.0880525528047,-5.40602226271004,2.68737815565284));
#32181=CARTESIAN_POINT('Ctrl Pts',(10.0626225986978,-5.4313856157096,2.64147803497406));
#32182=CARTESIAN_POINT('Ctrl Pts',(10.0378106134104,-5.45616506946334,2.59511401301077));
#32183=CARTESIAN_POINT('Ctrl Pts',(10.0365977316305,-5.45737636100752,2.59284760519095));
#32184=CARTESIAN_POINT('Ctrl Pts',(10.0353862170746,-5.45858636532748,2.59057995299073));
#32185=CARTESIAN_POINT('Ctrl Pts',(10.0341760716815,-5.45979507992655,2.58831105458924));
#32186=CARTESIAN_POINT('Ctrl Pts',(9.95003053478619,-5.5438411288367,2.43054680968724));
#32187=CARTESIAN_POINT('Ctrl Pts',(9.8724914512197,-5.62166228484852,2.26673902468443));
#32188=CARTESIAN_POINT('Ctrl Pts',(9.80219890345532,-5.69242165537877,2.09619946068861));
#32189=CARTESIAN_POINT('Ctrl Pts',(9.78976068958939,-5.70494247318471,2.06602261211724));
#32190=CARTESIAN_POINT('Ctrl Pts',(9.77754944575023,-5.71724209384684,2.03563491622785));
#32191=CARTESIAN_POINT('Ctrl Pts',(9.76556881474159,-5.72931576830717,2.00503247004604));
#32192=CARTESIAN_POINT('Ctrl Pts',(9.76544315633477,-5.72944240259681,2.00471149741701));
#32193=CARTESIAN_POINT('Ctrl Pts',(9.76531752303618,-5.72956901230779,2.00439049834638));
#32194=CARTESIAN_POINT('Ctrl Pts',(9.76519191485892,-5.72969559742598,2.00406947285931));
#32195=CARTESIAN_POINT('Ctrl Pts',(9.71400487072874,-5.78128075829942,1.87324721166454));
#32196=CARTESIAN_POINT('Ctrl Pts',(9.66697657534716,-5.82879541599935,1.73799752918786));
#32197=CARTESIAN_POINT('Ctrl Pts',(9.6250405522746,-5.87123312917844,1.60016514616698));
#32198=CARTESIAN_POINT('Ctrl Pts',(9.60161439240009,-5.89493954148945,1.52316968489148));
#32199=CARTESIAN_POINT('Ctrl Pts',(9.57977711929352,-5.91706181821158,1.44536936046407));
#32200=CARTESIAN_POINT('Ctrl Pts',(9.55968917829128,-5.93742663805485,1.36709188665601));
#32201=CARTESIAN_POINT('Ctrl Pts',(9.55947516461635,-5.93764360155217,1.36625793110865));
#32202=CARTESIAN_POINT('Ctrl Pts',(9.55926134903044,-5.93786036608929,1.36542391969325));
#32203=CARTESIAN_POINT('Ctrl Pts',(9.55904773172286,-5.93807693146144,1.36458985278468));
#32204=CARTESIAN_POINT('Ctrl Pts',(9.50331705704126,-5.99457672747216,1.1469899210633));
#32205=CARTESIAN_POINT('Ctrl Pts',(9.46041989832733,-6.0381883908994,0.924289620191035));
#32206=CARTESIAN_POINT('Ctrl Pts',(9.43130753977526,-6.06780345239864,0.696118554534736));
#32207=CARTESIAN_POINT('Ctrl Pts',(9.43114806151225,-6.06796568448157,0.694868627458047));
#32208=CARTESIAN_POINT('Ctrl Pts',(9.43098899634983,-6.06812749717018,0.693618531424424));
#32209=CARTESIAN_POINT('Ctrl Pts',(9.43083034447406,-6.06828889025085,0.69236826651728));
#32210=CARTESIAN_POINT('Ctrl Pts',(9.41547288739991,-6.08391169519064,0.571342974191852));
#32211=CARTESIAN_POINT('Ctrl Pts',(9.40406058123609,-6.09552882987824,0.448312367480381));
#32212=CARTESIAN_POINT('Ctrl Pts',(9.39675231043817,-6.10297030911209,0.324915545562507));
#32213=CARTESIAN_POINT('Ctrl Pts',(9.39030112011018,-6.10953908580177,0.215990136793151));
#32214=CARTESIAN_POINT('Ctrl Pts',(9.38704741662975,-6.11285457215368,0.106780944007842));
#32215=CARTESIAN_POINT('Ctrl Pts',(9.38707711882443,-6.11282361448583,-0.00157937270664588));
#32216=CARTESIAN_POINT('Ctrl Pts',(9.38707738015422,-6.11282334210997,-0.00253276283819925));
#32217=CARTESIAN_POINT('Ctrl Pts',(9.38707789550786,-6.1128228109299,-0.00348609118645972));
#32218=CARTESIAN_POINT('Ctrl Pts',(9.38707866494222,-6.11282202088418,-0.00443935704251815));
#32219=CARTESIAN_POINT('Ctrl Pts',(9.3872654421285,-6.11263024037226,-0.235840921054131));
#32220=CARTESIAN_POINT('Ctrl Pts',(9.40199748120688,-6.09761913563677,-0.465515426606816));
#32221=CARTESIAN_POINT('Ctrl Pts',(9.4309684633591,-6.06814824803631,-0.693455868487982));
#32222=CARTESIAN_POINT('Ctrl Pts',(9.43106885022933,-6.06804612895199,-0.694245701136398));
#32223=CARTESIAN_POINT('Ctrl Pts',(9.43116940824751,-6.06794383609246,-0.695035514567625));
#32224=CARTESIAN_POINT('Ctrl Pts',(9.43127013739879,-6.06784136947459,-0.695825308751845));
#32225=CARTESIAN_POINT('Ctrl Pts',(9.44755402646091,-6.05127660131423,-0.823503549992644));
#32226=CARTESIAN_POINT('Ctrl Pts',(9.46849384706743,-6.02998478850161,-0.951092004927493));
#32227=CARTESIAN_POINT('Ctrl Pts',(9.49358748617142,-6.00450023692484,-1.07683420677694));
#32228=CARTESIAN_POINT('Ctrl Pts',(9.51331996418398,-5.98446036341089,-1.17571206275323));
#32229=CARTESIAN_POINT('Ctrl Pts',(9.53562010983275,-5.96182877448762,-1.27344794850474));
#32230=CARTESIAN_POINT('Ctrl Pts',(9.56023113615348,-5.93687782718841,-1.36920204958066));
#32231=CARTESIAN_POINT('Ctrl Pts',(9.56048990352749,-5.93661548578795,-1.37020883560263));
#32232=CARTESIAN_POINT('Ctrl Pts',(9.56074892743608,-5.93635288702437,-1.37121540719265));
#32233=CARTESIAN_POINT('Ctrl Pts',(9.56100820760137,-5.93609003119388,-1.37222176345421));
#32234=CARTESIAN_POINT('Ctrl Pts',(9.61696238254866,-5.87936420680227,-1.58939932601352));
#32235=CARTESIAN_POINT('Ctrl Pts',(9.68492647384057,-5.81058800718736,-1.7984972507641));
#32236=CARTESIAN_POINT('Ctrl Pts',(9.76373024102914,-5.73116881967472,-2.00032985222453));
#32237=CARTESIAN_POINT('Ctrl Pts',(9.76456463201257,-5.7303279124905,-2.00246689857179));
#32238=CARTESIAN_POINT('Ctrl Pts',(9.76540023933697,-5.72948581132656,-2.00460313210208));
#32239=CARTESIAN_POINT('Ctrl Pts',(9.76623706163906,-5.72864251781373,-2.0067385537552));
#32240=CARTESIAN_POINT('Ctrl Pts',(9.82523364578579,-5.66918970857808,-2.15728734163231));
#32241=CARTESIAN_POINT('Ctrl Pts',(9.89067957083013,-5.60339936653193,-2.30450833756059));
#32242=CARTESIAN_POINT('Ctrl Pts',(9.96126858557544,-5.53271401884161,-2.4466727459975));
#32243=CARTESIAN_POINT('Ctrl Pts',(9.98467942415214,-5.50927123145484,-2.49382155561435));
#32244=CARTESIAN_POINT('Ctrl Pts',(10.0086561730407,-5.48528979005206,-2.54041446084365));
#32245=CARTESIAN_POINT('Ctrl Pts',(10.0331518093073,-5.46082159602852,-2.58638921905928));
#32246=CARTESIAN_POINT('Ctrl Pts',(10.0352622179174,-5.45871355169039,-2.59035015008101));
#32247=CARTESIAN_POINT('Ctrl Pts',(10.0373764572102,-5.45660191865752,-2.59430645369377));
#32248=CARTESIAN_POINT('Ctrl Pts',(10.0394944974403,-5.45448672989252,-2.59825809134046));
#32249=CARTESIAN_POINT('Ctrl Pts',(10.1231772780924,-5.37091660929666,-2.75438544987707));
#32250=CARTESIAN_POINT('Ctrl Pts',(10.2123532673795,-5.28219670560045,-2.90302025346162));
#32251=CARTESIAN_POINT('Ctrl Pts',(10.3066428918801,-5.18899936326121,-3.04491648351723));
#32252=CARTESIAN_POINT('Ctrl Pts',(10.4047692317532,-5.09200975132797,-3.19258657734662));
#32253=CARTESIAN_POINT('Ctrl Pts',(10.5084338580352,-4.99017075072625,-3.33295843771009));
#32254=CARTESIAN_POINT('Ctrl Pts',(10.6172356637028,-4.88420776535908,-3.46684409098579));
#32255=CARTESIAN_POINT('Ctrl Pts',(10.6505136862934,-4.85179802179666,-3.50779423668353));
#32256=CARTESIAN_POINT('Ctrl Pts',(10.6842724713102,-4.81900226877546,-3.54813734782343));
#32257=CARTESIAN_POINT('Ctrl Pts',(10.718501004134,-4.78584072941129,-3.58789601986351));
#32258=CARTESIAN_POINT('Ctrl Pts',(10.7258311426537,-4.77873909060255,-3.59641045356464));
#32259=CARTESIAN_POINT('Ctrl Pts',(10.7331821298285,-4.77162136370932,-3.60489727595804));
#32260=CARTESIAN_POINT('Ctrl Pts',(10.7405539922153,-4.76448761189709,-3.6133568876269));
#32261=CARTESIAN_POINT('Ctrl Pts',(10.8109577635415,-4.69635787684114,-3.69414903134668));
#32262=CARTESIAN_POINT('Ctrl Pts',(10.8832920761415,-4.62673602708103,-3.77233650058384));
#32263=CARTESIAN_POINT('Ctrl Pts',(10.9573999400201,-4.55592983802426,-3.84797903420149));
#32264=CARTESIAN_POINT('Ctrl Pts',(11.0332070572439,-4.48350010124507,-3.92535601031363));
#32265=CARTESIAN_POINT('Ctrl Pts',(11.1108707017101,-4.40982991477362,-4.00007045807862));
#32266=CARTESIAN_POINT('Ctrl Pts',(11.1902510794477,-4.33523070780175,-4.07214227964421));
#32267=CARTESIAN_POINT('Ctrl Pts',(11.2682864139836,-4.26189553054412,-4.14299289621692));
#32268=CARTESIAN_POINT('Ctrl Pts',(11.3479816279103,-4.18766133326008,-4.21128986378364));
#32269=CARTESIAN_POINT('Ctrl Pts',(11.4292191118081,-4.11282480171223,-4.27700572216152));
#32270=CARTESIAN_POINT('Ctrl Pts',(11.4719750782119,-4.07343771000138,-4.31159252739222));
#32271=CARTESIAN_POINT('Ctrl Pts',(11.515158434596,-4.03388389452131,-4.34546356908915));
#32272=CARTESIAN_POINT('Ctrl Pts',(11.5587526034551,-3.99420842547088,-4.37860926807613));
#32273=CARTESIAN_POINT('Origin',(-3.88784034431744,0.,0.));
#32274=CARTESIAN_POINT('',(-2.88899111509131,-7.40661556618246E-16,6.04796058042142));
#32275=CARTESIAN_POINT('Origin',(-2.88899111509131,0.,0.));
#32276=CARTESIAN_POINT('',(-3.88784034431744,-6.0599836255502E-16,4.94835215326525));
#32277=CARTESIAN_POINT('',(-3.88784034431744,-6.0599836255502E-16,4.94835215326525));
#32278=CARTESIAN_POINT('Origin',(-3.88784034431744,0.,0.));
#32279=CARTESIAN_POINT('Origin',(18.3245838861624,0.,0.));
#32280=CARTESIAN_POINT('',(18.3706375907924,0.,-4.25614904904291));
#32281=CARTESIAN_POINT('',(18.5421134565937,0.,-4.27463759471298));
#32282=CARTESIAN_POINT('Origin',(18.3245838861624,0.,-5.48772230081581));
#32283=CARTESIAN_POINT('',(18.9788234605247,-4.08475030728679,-5.09745204146194));
#32284=CARTESIAN_POINT('Ctrl Pts',(18.5421134565937,-4.25668091127711E-16,
-4.27463759471298));
#32285=CARTESIAN_POINT('Ctrl Pts',(18.5421134565937,-0.0254801014594758,
-4.27463759471298));
#32286=CARTESIAN_POINT('Ctrl Pts',(18.5445357600052,-0.0504618671715304,
-4.27483896810787));
#32287=CARTESIAN_POINT('Ctrl Pts',(18.5488507525854,-0.0749847941031531,
-4.27520750677706));
#32288=CARTESIAN_POINT('Ctrl Pts',(18.5549572286634,-0.109689063899206,
-4.27572905403939));
#32289=CARTESIAN_POINT('Ctrl Pts',(18.5648536938036,-0.143474544424252,
-4.27659263523378));
#32290=CARTESIAN_POINT('Ctrl Pts',(18.577017371859,-0.176443360724415,-4.27778034521236));
#32291=CARTESIAN_POINT('Ctrl Pts',(18.5859098337359,-0.200545769612747,
-4.27864864061259));
#32292=CARTESIAN_POINT('Ctrl Pts',(18.5960132886523,-0.224211738802833,
-4.2796923434056));
#32293=CARTESIAN_POINT('Ctrl Pts',(18.6067345431864,-0.247476011988283,
-4.28087311968421));
#32294=CARTESIAN_POINT('Ctrl Pts',(18.6106785062611,-0.256034099487255,
-4.28130748471373));
#32295=CARTESIAN_POINT('Ctrl Pts',(18.6147061344625,-0.264537763086523,
-4.2817599332196));
#32296=CARTESIAN_POINT('Ctrl Pts',(18.6187881934998,-0.272988456681822,
-4.28222671824238));
#32297=CARTESIAN_POINT('Ctrl Pts',(18.6338157474098,-0.304098553920046,
-4.28394512481861));
#32298=CARTESIAN_POINT('Ctrl Pts',(18.6497999181611,-0.334819746905005,
-4.28589352869452));
#32299=CARTESIAN_POINT('Ctrl Pts',(18.6663913361296,-0.365265144948759,
-4.28810690858487));
#32300=CARTESIAN_POINT('Ctrl Pts',(18.6822196269575,-0.394310197971121,
-4.29021848341734));
#32301=CARTESIAN_POINT('Ctrl Pts',(18.6986002223778,-0.423104522276839,
-4.29257138621942));
#32302=CARTESIAN_POINT('Ctrl Pts',(18.7152343269478,-0.451742333789593,
-4.29514932713806));
#32303=CARTESIAN_POINT('Ctrl Pts',(18.7288317921048,-0.475152168841498,
-4.29725665198207));
#32304=CARTESIAN_POINT('Ctrl Pts',(18.742598638901,-0.498457416161126,-4.29951352128347));
#32305=CARTESIAN_POINT('Ctrl Pts',(18.7563766796154,-0.521705510096399,
-4.30188582063063));
#32306=CARTESIAN_POINT('Ctrl Pts',(18.783169802229,-0.566914335084774,-4.30649905328121));
#32307=CARTESIAN_POINT('Ctrl Pts',(18.8101446723159,-0.611979171936971,
-4.31158867889594));
#32308=CARTESIAN_POINT('Ctrl Pts',(18.8370689932334,-0.657009298536488,
-4.31718836948623));
#32309=CARTESIAN_POINT('Ctrl Pts',(18.8638321278848,-0.701769845896118,
-4.32275453673455));
#32310=CARTESIAN_POINT('Ctrl Pts',(18.890544823512,-0.746496520158024,-4.3288246153777));
#32311=CARTESIAN_POINT('Ctrl Pts',(18.9169838610535,-0.791287166948651,
-4.33538155269578));
#32312=CARTESIAN_POINT('Ctrl Pts',(18.943298883484,-0.835867718457729,-4.34190773400361));
#32313=CARTESIAN_POINT('Ctrl Pts',(18.9693423170444,-0.880512000020209,
-4.34891600802757));
#32314=CARTESIAN_POINT('Ctrl Pts',(18.9949063476124,-0.925301239209109,
-4.35634180429196));
#32315=CARTESIAN_POINT('Ctrl Pts',(19.0109806429501,-0.953464069665662,
-4.36101103835323));
#32316=CARTESIAN_POINT('Ctrl Pts',(19.0268656680106,-0.981683884269773,
-4.36584439788146));
#32317=CARTESIAN_POINT('Ctrl Pts',(19.042513570575,-1.00997688847436,-4.37081681177666));
#32318=CARTESIAN_POINT('Ctrl Pts',(19.0798137917417,-1.07741949363883,-4.38266965513763));
#32319=CARTESIAN_POINT('Ctrl Pts',(19.1158787124396,-1.14523365849758,-4.39540379894711));
#32320=CARTESIAN_POINT('Ctrl Pts',(19.1504383167282,-1.21359345665619,-4.4089470513481));
#32321=CARTESIAN_POINT('Ctrl Pts',(19.1844668878412,-1.28090285735068,-4.42228220193544));
#32322=CARTESIAN_POINT('Ctrl Pts',(19.2170359214768,-1.34874153614133,-4.43640163180863));
#32323=CARTESIAN_POINT('Ctrl Pts',(19.2478784152531,-1.41724208592662,-4.45119997195958));
#32324=CARTESIAN_POINT('Ctrl Pts',(19.2618719954876,-1.44832154229253,-4.45791414240713));
#32325=CARTESIAN_POINT('Ctrl Pts',(19.2755100453659,-1.47953675967748,-4.46476758171775));
#32326=CARTESIAN_POINT('Ctrl Pts',(19.2887671097419,-1.51089754629334,-4.47174804387616));
#32327=CARTESIAN_POINT('Ctrl Pts',(19.3157307639414,-1.57468251268946,-4.48594566428848));
#32328=CARTESIAN_POINT('Ctrl Pts',(19.3411921421037,-1.63922105464934,-4.50071861138956));
#32329=CARTESIAN_POINT('Ctrl Pts',(19.3648781089758,-1.70442847903499,-4.51596285581109));
#32330=CARTESIAN_POINT('Ctrl Pts',(19.3879193855577,-1.76786107220608,-4.53079217875556));
#32331=CARTESIAN_POINT('Ctrl Pts',(19.4092802005646,-1.83192674775908,-4.54606702186589));
#32332=CARTESIAN_POINT('Ctrl Pts',(19.4287217645248,-1.89650177828534,-4.5616800383172));
#32333=CARTESIAN_POINT('Ctrl Pts',(19.4427734845,-1.94317447643887,-4.57296461066907));
#32334=CARTESIAN_POINT('Ctrl Pts',(19.4558228421615,-1.9901123111244,-4.58442557886488));
#32335=CARTESIAN_POINT('Ctrl Pts',(19.4677856588679,-2.03725270625742,-4.59602059784627));
#32336=CARTESIAN_POINT('Ctrl Pts',(19.4836157479168,-2.09963238414392,-4.61136398958295));
#32337=CARTESIAN_POINT('Ctrl Pts',(19.4975218504262,-2.16228822832006,-4.62690576465906));
#32338=CARTESIAN_POINT('Ctrl Pts',(19.5093789068896,-2.22527395400374,-4.64262367122429));
#32339=CARTESIAN_POINT('Ctrl Pts',(19.5206604386916,-2.28520244212082,-4.65757865295381));
#32340=CARTESIAN_POINT('Ctrl Pts',(19.5300868182461,-2.34542993100449,-4.67269369206331));
#32341=CARTESIAN_POINT('Ctrl Pts',(19.5375083329815,-2.40599268770172,-4.68793464693561));
#32342=CARTESIAN_POINT('Ctrl Pts',(19.5447205451536,-2.46484744533578,-4.70274577433533));
#32343=CARTESIAN_POINT('Ctrl Pts',(19.5500392215662,-2.52401927226447,-4.71767635525021));
#32344=CARTESIAN_POINT('Ctrl Pts',(19.5532886451223,-2.58352585445992,-4.73267227407408));
#32345=CARTESIAN_POINT('Ctrl Pts',(19.5568715014676,-2.64913857989318,-4.74920696768458));
#32346=CARTESIAN_POINT('Ctrl Pts',(19.5579208431573,-2.71488993281246,-4.76576752417364));
#32347=CARTESIAN_POINT('Ctrl Pts',(19.5562274234509,-2.78054074813488,-4.78226180213361));
#32348=CARTESIAN_POINT('Ctrl Pts',(19.5545894883089,-2.84404052737642,-4.79821564831301));
#32349=CARTESIAN_POINT('Ctrl Pts',(19.5503851390046,-2.90744624410649,-4.81410756418141));
#32350=CARTESIAN_POINT('Ctrl Pts',(19.543432946332,-2.97049514836484,-4.82984508554704));
#32351=CARTESIAN_POINT('Ctrl Pts',(19.537295918086,-3.0261513887096,-4.84373733763073));
#32352=CARTESIAN_POINT('Ctrl Pts',(19.5290174995114,-3.08152901217754,-4.85750921071767));
#32353=CARTESIAN_POINT('Ctrl Pts',(19.5184828236628,-3.13641568626229,-4.87109011242972));
#32354=CARTESIAN_POINT('Ctrl Pts',(19.5095221706226,-3.18310155017265,-4.88264184406006));
#32355=CARTESIAN_POINT('Ctrl Pts',(19.4989688849651,-3.22928780844808,-4.89398417428052));
#32356=CARTESIAN_POINT('Ctrl Pts',(19.4867363354049,-3.27496260554755,-4.90515615271697));
#32357=CARTESIAN_POINT('Ctrl Pts',(19.4747569202957,-3.31969223053607,-4.91609694364712));
#32358=CARTESIAN_POINT('Ctrl Pts',(19.461166645143,-3.36393186154866,-4.92687481197273));
#32359=CARTESIAN_POINT('Ctrl Pts',(19.4458481150729,-3.40765453681482,-4.93749794545092));
#32360=CARTESIAN_POINT('Ctrl Pts',(19.4309480706269,-3.45018275602269,-4.94783086644636));
#32361=CARTESIAN_POINT('Ctrl Pts',(19.4144124535007,-3.49222233510551,-4.958017738087));
#32362=CARTESIAN_POINT('Ctrl Pts',(19.3961048908036,-3.53372627849561,-4.96803313457627));
#32363=CARTESIAN_POINT('Ctrl Pts',(19.3777973281065,-3.57523022188571,-4.97804853106554));
#32364=CARTESIAN_POINT('Ctrl Pts',(19.3577173695828,-3.61619911705965,-4.98789295307204));
#32365=CARTESIAN_POINT('Ctrl Pts',(19.3357063971287,-3.65655558431263,-4.99750105264302));
#32366=CARTESIAN_POINT('Ctrl Pts',(19.313266779319,-3.69769796015238,-5.00729626195055));
#32367=CARTESIAN_POINT('Ctrl Pts',(19.289134021862,-3.73764489679991,-5.01669780151543));
#32368=CARTESIAN_POINT('Ctrl Pts',(19.2632223927464,-3.7762889522877,-5.02575304016386));
#32369=CARTESIAN_POINT('Ctrl Pts',(19.2390742535079,-3.8123029762803,-5.03419199870034));
#32370=CARTESIAN_POINT('Ctrl Pts',(19.2133802940762,-3.84718564933888,-5.04233026248691));
#32371=CARTESIAN_POINT('Ctrl Pts',(19.1860503642663,-3.8808244610573,-5.05017035603905));
#32372=CARTESIAN_POINT('Ctrl Pts',(19.1594485534184,-3.91356707374257,-5.05780157526114));
#32373=CARTESIAN_POINT('Ctrl Pts',(19.1312961252711,-3.94513151564625,-5.06515054788063));
#32374=CARTESIAN_POINT('Ctrl Pts',(19.1014999739291,-3.9753850188093,-5.0721818065022));
#32375=CARTESIAN_POINT('Ctrl Pts',(19.0728862687923,-4.00443792597597,-5.07893403294343));
#32376=CARTESIAN_POINT('Ctrl Pts',(19.0427560661447,-4.03228200530944,-5.08539335384616));
#32377=CARTESIAN_POINT('Ctrl Pts',(19.0110269646178,-4.05876964694868,-5.09149074847995));
#32378=CARTESIAN_POINT('Ctrl Pts',(19.0004703578505,-4.0675823647227,-5.09351941599201));
#32379=CARTESIAN_POINT('Ctrl Pts',(18.9897368016208,-4.07624466766795,-5.095507695138));
#32380=CARTESIAN_POINT('Ctrl Pts',(18.9788234605247,-4.08475030728679,-5.09745204146194));
#32381=CARTESIAN_POINT('',(18.9788234605247,-4.08475030728679,5.09745204146194));
#32382=CARTESIAN_POINT('Origin',(18.9788234605247,0.,0.));
#32383=CARTESIAN_POINT('',(18.5421134565937,0.,4.27463759471298));
#32384=CARTESIAN_POINT('Ctrl Pts',(18.9788234605247,-4.08475030728679,5.09745204146194));
#32385=CARTESIAN_POINT('Ctrl Pts',(19.0092155017241,-4.06106335867525,5.09203732445985));
#32386=CARTESIAN_POINT('Ctrl Pts',(19.038201878942,-4.03614678048446,5.08630814962051));
#32387=CARTESIAN_POINT('Ctrl Pts',(19.0658854085647,-4.01010768196352,5.08030731363521));
#32388=CARTESIAN_POINT('Ctrl Pts',(19.0945031333629,-3.98318988045413,5.07410397630336));
#32389=CARTESIAN_POINT('Ctrl Pts',(19.1217292974,-3.95507228369758,5.06761017514692));
#32390=CARTESIAN_POINT('Ctrl Pts',(19.1476684840898,-3.92584011263657,5.0608292638313));
#32391=CARTESIAN_POINT('Ctrl Pts',(19.1587650009721,-3.91333489095928,5.05792845981647));
#32392=CARTESIAN_POINT('Ctrl Pts',(19.1696258235112,-3.90062531636491,5.05497459316725));
#32393=CARTESIAN_POINT('Ctrl Pts',(19.180258194112,-3.88771648264067,5.05196571294776));
#32394=CARTESIAN_POINT('Ctrl Pts',(19.2038753205281,-3.85904276824554,5.045282245339));
#32395=CARTESIAN_POINT('Ctrl Pts',(19.2264219802684,-3.82928334263606,5.03832874515852));
#32396=CARTESIAN_POINT('Ctrl Pts',(19.2477875023842,-3.79870511095283,5.03114432286621));
#32397=CARTESIAN_POINT('Ctrl Pts',(19.2693156963375,-3.76789406412439,5.02390520014726));
#32398=CARTESIAN_POINT('Ctrl Pts',(19.2896444858868,-3.73625219157716,5.01643186588051));
#32399=CARTESIAN_POINT('Ctrl Pts',(19.3087047767471,-3.70405870503921,5.0087932128783));
#32400=CARTESIAN_POINT('Ctrl Pts',(19.3184086433773,-3.68766854069105,5.00490426540574));
#32401=CARTESIAN_POINT('Ctrl Pts',(19.3277844439617,-3.67113545045191,5.00097290629788));
#32402=CARTESIAN_POINT('Ctrl Pts',(19.3368275939036,-3.65449625972552,4.99701072297555));
#32403=CARTESIAN_POINT('Ctrl Pts',(19.363374077786,-3.60565133165635,4.98537959484204));
#32404=CARTESIAN_POINT('Ctrl Pts',(19.3873130954724,-3.55545669304448,4.97334289549462));
#32405=CARTESIAN_POINT('Ctrl Pts',(19.4087322482119,-3.50426728284812,4.96099350117674));
#32406=CARTESIAN_POINT('Ctrl Pts',(19.4306743089924,-3.45182818016717,4.94834261978939));
#32407=CARTESIAN_POINT('Ctrl Pts',(19.4499725786457,-3.39834527030435,4.93536346761216));
#32408=CARTESIAN_POINT('Ctrl Pts',(19.4667506470085,-3.34415611304767,4.92213926982721));
#32409=CARTESIAN_POINT('Ctrl Pts',(19.4841244237279,-3.28804295994605,4.9084455445043));
#32410=CARTESIAN_POINT('Ctrl Pts',(19.4987964466969,-3.23117263090285,4.89448894356967));
#32411=CARTESIAN_POINT('Ctrl Pts',(19.5109258361256,-3.17387129428592,4.88034611034631));
#32412=CARTESIAN_POINT('Ctrl Pts',(19.5139266235123,-3.15969505489859,4.87684720087532));
#32413=CARTESIAN_POINT('Ctrl Pts',(19.5167718648232,-3.14549220605671,4.87333682487201));
#32414=CARTESIAN_POINT('Ctrl Pts',(19.5194641043032,-3.13126724135225,4.86981601487401));
#32415=CARTESIAN_POINT('Ctrl Pts',(19.5310219267275,-3.07019926531775,4.85470112741758));
#32416=CARTESIAN_POINT('Ctrl Pts',(19.5397754782162,-3.00866440890858,4.83935864683886));
#32417=CARTESIAN_POINT('Ctrl Pts',(19.5459099142417,-2.94691930253355,4.82389985356588));
#32418=CARTESIAN_POINT('Ctrl Pts',(19.5522227928369,-2.88337811329133,4.80799138459591));
#32419=CARTESIAN_POINT('Ctrl Pts',(19.5557625400972,-2.81961415152491,4.7919596033858));
#32420=CARTESIAN_POINT('Ctrl Pts',(19.5567380782345,-2.75585562629362,4.77590586845312));
#32421=CARTESIAN_POINT('Ctrl Pts',(19.5577584028666,-2.68916997730747,4.75911511413825));
#32422=CARTESIAN_POINT('Ctrl Pts',(19.5559742312122,-2.62249021315083,4.74230020891914));
#32423=CARTESIAN_POINT('Ctrl Pts',(19.5516233603138,-2.55602310574085,4.72555767462613));
#32424=CARTESIAN_POINT('Ctrl Pts',(19.5471598377419,-2.48783504842201,4.70838164677534));
#32425=CARTESIAN_POINT('Ctrl Pts',(19.5399954701845,-2.41987049650095,4.69128154228306));
#32426=CARTESIAN_POINT('Ctrl Pts',(19.5303775138833,-2.35229992639511,4.6743446041456));
#32427=CARTESIAN_POINT('Ctrl Pts',(19.520376925709,-2.28204119125675,4.6567338625344));
#32428=CARTESIAN_POINT('Ctrl Pts',(19.507724084395,-2.21220816070646,4.63929926101361));
#32429=CARTESIAN_POINT('Ctrl Pts',(19.492679467708,-2.14294033361043,4.62212469053316));
#32430=CARTESIAN_POINT('Ctrl Pts',(19.4850149126374,-2.10765149332649,4.61337501987018));
#32431=CARTESIAN_POINT('Ctrl Pts',(19.4767292665588,-2.0725085539897,4.60469264187981));
#32432=CARTESIAN_POINT('Ctrl Pts',(19.4678548462165,-2.03752539429306,4.5960876712563));
#32433=CARTESIAN_POINT('Ctrl Pts',(19.4506703711719,-1.96978381663498,4.5794249600892));
#32434=CARTESIAN_POINT('Ctrl Pts',(19.4312143025218,-1.90239275960969,4.56299625837018));
#32435=CARTESIAN_POINT('Ctrl Pts',(19.4097043313689,-1.83546262513185,4.54693533472414));
#32436=CARTESIAN_POINT('Ctrl Pts',(19.3868675723589,-1.76440407555393,4.52988373385595));
#32437=CARTESIAN_POINT('Ctrl Pts',(19.3617159606843,-1.69386543536571,4.5132472326653));
#32438=CARTESIAN_POINT('Ctrl Pts',(19.334527787239,-1.62391968717625,4.49717291690614));
#32439=CARTESIAN_POINT('Ctrl Pts',(19.3080958649913,-1.55591951123851,4.48154571542506));
#32440=CARTESIAN_POINT('Ctrl Pts',(19.2797395402235,-1.48847914543718,4.46645016856151));
#32441=CARTESIAN_POINT('Ctrl Pts',(19.2497252658693,-1.42161421705033,4.45200331335871));
#32442=CARTESIAN_POINT('Ctrl Pts',(19.2184228711861,-1.35187965161869,4.43693644357022));
#32443=CARTESIAN_POINT('Ctrl Pts',(19.1853175219329,-1.28277087816504,4.42257571144363));
#32444=CARTESIAN_POINT('Ctrl Pts',(19.1507173950585,-1.21425305164681,4.40902684453694));
#32445=CARTESIAN_POINT('Ctrl Pts',(19.1161172681841,-1.14573522512858,4.39547797763025));
#32446=CARTESIAN_POINT('Ctrl Pts',(19.0800227461583,-1.07780776258487,4.38274130761694));
#32447=CARTESIAN_POINT('Ctrl Pts',(19.0427420848227,-1.01039009749801,4.37088944250479));
#32448=CARTESIAN_POINT('Ctrl Pts',(19.0176862009639,-0.965079496078312,
4.36292394658491));
#32449=CARTESIAN_POINT('Ctrl Pts',(18.9920359319277,-0.919985408305112,
4.35532184851541));
#32450=CARTESIAN_POINT('Ctrl Pts',(18.9659876672824,-0.875027301247306,
4.34817500505906));
#32451=CARTESIAN_POINT('Ctrl Pts',(18.9398815492249,-0.829969341860113,
4.34101228840401));
#32452=CARTESIAN_POINT('Ctrl Pts',(18.9133761474955,-0.785047651405376,
4.33430711611102));
#32453=CARTESIAN_POINT('Ctrl Pts',(18.8866851821932,-0.740163271093601,
4.32810525027266));
#32454=CARTESIAN_POINT('Ctrl Pts',(18.8597891825343,-0.694934098454789,
4.32185574301118));
#32455=CARTESIAN_POINT('Ctrl Pts',(18.8327052521153,-0.649742429280504,
4.31611747411665));
#32456=CARTESIAN_POINT('Ctrl Pts',(18.8056609345573,-0.604474127390862,
4.31088651744545));
#32457=CARTESIAN_POINT('Ctrl Pts',(18.789219980108,-0.576954331863708,4.30770648081951));
#32458=CARTESIAN_POINT('Ctrl Pts',(18.7727938031056,-0.54940598728245,4.30471292813371));
#32459=CARTESIAN_POINT('Ctrl Pts',(18.7564339386911,-0.521802123955709,
4.30189568020001));
#32460=CARTESIAN_POINT('Ctrl Pts',(18.7397027696494,-0.49357176141591,4.29901449181013));
#32461=CARTESIAN_POINT('Ctrl Pts',(18.7229895518091,-0.465269352172632,
4.29630414918437));
#32462=CARTESIAN_POINT('Ctrl Pts',(18.7065689069815,-0.436780695224228,
4.29382139179048));
#32463=CARTESIAN_POINT('Ctrl Pts',(18.6895291685526,-0.407217954681067,
4.2912450291069));
#32464=CARTESIAN_POINT('Ctrl Pts',(18.6728048477287,-0.377454401795733,
4.28891382372324));
#32465=CARTESIAN_POINT('Ctrl Pts',(18.6567126558758,-0.34735464947781,4.28683470028683));
#32466=CARTESIAN_POINT('Ctrl Pts',(18.6435340824926,-0.322704695117279,
4.28513201857449));
#32467=CARTESIAN_POINT('Ctrl Pts',(18.6307797349848,-0.297829040646783,
4.28359715999337));
#32468=CARTESIAN_POINT('Ctrl Pts',(18.6186255330937,-0.272651611164468,
4.28220812332119));
#32469=CARTESIAN_POINT('Ctrl Pts',(18.6073623729794,-0.249319974742047,
4.28092091889726));
#32470=CARTESIAN_POINT('Ctrl Pts',(18.5965521051593,-0.225577884414913,
4.27975640143456));
#32471=CARTESIAN_POINT('Ctrl Pts',(18.5867835955735,-0.201439120566317,
4.27876353217638));
#32472=CARTESIAN_POINT('Ctrl Pts',(18.5737591691624,-0.169254727375367,
4.2774397322174));
#32473=CARTESIAN_POINT('Ctrl Pts',(18.5625877203779,-0.13636500536244,4.2764190207263));
#32474=CARTESIAN_POINT('Ctrl Pts',(18.5546757430905,-0.102787459871969,
4.27572220356722));
#32475=CARTESIAN_POINT('Ctrl Pts',(18.5488806896841,-0.0781939022432147,
4.27521182638783));
#32476=CARTESIAN_POINT('Ctrl Pts',(18.5448346783279,-0.0532311433030454,
4.27487102240903));
#32477=CARTESIAN_POINT('Ctrl Pts',(18.5430852251124,-0.0279031173504605,
4.27472118600104));
#32478=CARTESIAN_POINT('Ctrl Pts',(18.5424461526085,-0.0186508293669923,
4.27466645099722));
#32479=CARTESIAN_POINT('Ctrl Pts',(18.5421134565937,-0.00934977220112235,
4.27463759471298));
#32480=CARTESIAN_POINT('Ctrl Pts',(18.5421134565937,0.,4.27463759471298));
#32481=CARTESIAN_POINT('',(18.3706375907924,0.,4.25614904904291));
#32482=CARTESIAN_POINT('Origin',(18.3245838861624,0.,5.48772230081581));
#32483=CARTESIAN_POINT('Origin',(18.3706375907924,0.,0.));
#32484=CARTESIAN_POINT('Origin',(14.8870768733179,0.,0.));
#32485=CARTESIAN_POINT('Origin',(14.8870768733179,0.,0.));
#32486=CARTESIAN_POINT('Origin',(11.1121596556826,0.,0.));
#32487=CARTESIAN_POINT('Origin',(14.8870768733179,0.,0.));
#32488=CARTESIAN_POINT('Origin',(-60.4312629272455,0.,0.));
#32489=CARTESIAN_POINT('',(-3.88784034431744,-4.89858719658941E-16,-4.));
#32490=CARTESIAN_POINT('',(-60.4312629272455,-4.89858719658941E-16,-4.));
#32491=CARTESIAN_POINT('Origin',(-3.88784034431744,0.,0.));
#32492=CARTESIAN_POINT('Origin',(11.1121596556826,0.,0.));
#32493=CARTESIAN_POINT('',(11.1121596556826,-8.22991738629016E-16,6.72023753462643));
#32494=CARTESIAN_POINT('Origin',(11.1121596556826,0.,0.));
#32495=CARTESIAN_POINT('',(11.1121596556826,-8.22991738629016E-16,6.72023753462643));
#32496=CARTESIAN_POINT('',(11.1121596556826,-4.27128032554705,-5.18823254127999));
#32497=CARTESIAN_POINT('Origin',(11.1121596556826,0.,0.));
#32498=CARTESIAN_POINT('',(11.1585526803519,-4.38134327770265,-5.09856534401068));
#32499=CARTESIAN_POINT('Ctrl Pts',(11.1121596556826,-4.27128032554706,-5.18823254127999));
#32500=CARTESIAN_POINT('Ctrl Pts',(11.1121596556826,-4.27665349298167,-5.18380901088371));
#32501=CARTESIAN_POINT('Ctrl Pts',(11.1124205603573,-4.2820265275568,-5.17938779583192));
#32502=CARTESIAN_POINT('Ctrl Pts',(11.1153502651155,-4.31100162102884,-5.15556504699343));
#32503=CARTESIAN_POINT('Ctrl Pts',(11.1231194250036,-4.33370705720515,-5.13696310729952));
#32504=CARTESIAN_POINT('Ctrl Pts',(11.143213732739,-4.36424955048543,-5.11225066055275));
#32505=CARTESIAN_POINT('Ctrl Pts',(11.1504180869028,-4.37306471988177,-5.10516435342262));
#32506=CARTESIAN_POINT('Ctrl Pts',(11.1585526803519,-4.38134327770264,-5.09856534401069));
#32507=CARTESIAN_POINT('Ctrl Pts',(11.1585526803519,-4.38134327770267,-5.09856534401067));
#32508=CARTESIAN_POINT('Ctrl Pts',(10.8280078030872,-4.68201126458796,-4.8192662818435));
#32509=CARTESIAN_POINT('Ctrl Pts',(10.5214494479963,-4.97337279470518,-4.49935967199326));
#32510=CARTESIAN_POINT('Ctrl Pts',(9.97229944890177,-5.50399269762474,-3.78583316881013));
#32511=CARTESIAN_POINT('Ctrl Pts',(9.72884798379595,-5.74433681300753,-3.39271619660671));
#32512=CARTESIAN_POINT('Ctrl Pts',(9.31382031628678,-6.15730438613379,-2.51609523661562));
#32513=CARTESIAN_POINT('Ctrl Pts',(9.14962517763389,-6.32266022732949,-2.04686959132891));
#32514=CARTESIAN_POINT('Ctrl Pts',(8.97968417042009,-6.49418647715621,-1.29879006759369));
#32515=CARTESIAN_POINT('Ctrl Pts',(8.93575384240423,-6.53864733931865,-1.04005934340375));
#32516=CARTESIAN_POINT('Ctrl Pts',(8.87777246418902,-6.59736187089493,-0.523086822034743));
#32517=CARTESIAN_POINT('Ctrl Pts',(8.8631452526061,-6.61219755450612,-0.263005427051395));
#32518=CARTESIAN_POINT('Ctrl Pts',(8.86304815521195,-6.6122959841467,0.260400685698262));
#32519=CARTESIAN_POINT('Ctrl Pts',(8.87795718231789,-6.59717455971195,0.525795200917309));
#32520=CARTESIAN_POINT('Ctrl Pts',(8.93628291242789,-6.53811183992734,1.04370213362036));
#32521=CARTESIAN_POINT('Ctrl Pts',(8.97946099290913,-6.49441229642004,1.29752474849125));
#32522=CARTESIAN_POINT('Ctrl Pts',(9.09245107359478,-6.38036710627489,1.79547047261785));
#32523=CARTESIAN_POINT('Ctrl Pts',(9.16291409861826,-6.3093667473441,2.0412446593706));
#32524=CARTESIAN_POINT('Ctrl Pts',(9.32652223254246,-6.14517355622585,2.51312695721537));
#32525=CARTESIAN_POINT('Ctrl Pts',(9.41946362141348,-6.05218100166854,2.73949361055882));
#32526=CARTESIAN_POINT('Ctrl Pts',(9.62584947135055,-5.84682859048649,3.17490081246898));
#32527=CARTESIAN_POINT('Ctrl Pts',(9.73996892072135,-5.73380090596656,3.38497438741758));
#32528=CARTESIAN_POINT('Ctrl Pts',(9.98471062769431,-5.49326410523417,3.78353127448484));
#32529=CARTESIAN_POINT('Ctrl Pts',(10.1146920373345,-5.36637373914797,3.97129991678004));
#32530=CARTESIAN_POINT('Ctrl Pts',(10.5258167104531,-4.96921689661331,4.50410582808353));
#32531=CARTESIAN_POINT('Ctrl Pts',(10.828058423632,-4.68196521947166,4.81930905446431));
#32532=CARTESIAN_POINT('Ctrl Pts',(11.1585526803519,-4.38134327770267,5.09856534401067));
#32533=CARTESIAN_POINT('Origin',(14.8870768733179,0.,0.));
#32534=CARTESIAN_POINT('',(18.7837086993174,-4.27128032554705,-5.09745204146194));
#32535=CARTESIAN_POINT('Origin',(14.8870768733179,0.,-5.09745204146194));
#32536=CARTESIAN_POINT('',(14.8870768733179,-4.27128032554705,-6.41621047834285));
#32537=CARTESIAN_POINT('Origin',(14.8870768733179,-4.27128032554705,0.));
#32538=CARTESIAN_POINT('',(14.8870768733179,-4.71972237234598E-16,-7.70789157434132));
#32539=CARTESIAN_POINT('Origin',(14.8870768733179,0.,0.));
#32540=CARTESIAN_POINT('Origin',(14.8870768733179,-4.27128032554705,0.));
#32541=CARTESIAN_POINT('',(14.8870768733179,-4.71972237234598E-16,7.70789157434132));
#32542=CARTESIAN_POINT('Origin',(14.8870768733179,0.,0.));
#32543=CARTESIAN_POINT('Origin',(14.8870768733179,0.,5.09745204146194));
#32544=CARTESIAN_POINT('Origin',(-3.88784034431744,6.,0.));
#32545=CARTESIAN_POINT('Origin',(18.3575990203927,-10.,4.26678755349543));
#32546=CARTESIAN_POINT('',(18.4538614420533,0.,4.26678755349543));
#32547=CARTESIAN_POINT('',(18.3575990203927,0.,4.26678755349543));
#32548=CARTESIAN_POINT('',(18.7133976597241,-3.81977834524697,4.26678755349543));
#32549=CARTESIAN_POINT('Ctrl Pts',(18.4538614420644,-2.56528132069889E-12,
4.26678755349543));
#32550=CARTESIAN_POINT('Ctrl Pts',(18.4538614420546,-0.0764186347087233,
4.26678755349543));
#32551=CARTESIAN_POINT('Ctrl Pts',(18.4647576002876,-0.151683565594343,
4.266787553495));
#32552=CARTESIAN_POINT('Ctrl Pts',(18.4806164604976,-0.225114443517557,
4.26678755349578));
#32553=CARTESIAN_POINT('Ctrl Pts',(18.4822477496512,-0.232667760282275,
4.26678755349586));
#32554=CARTESIAN_POINT('Ctrl Pts',(18.4839315235274,-0.240201701574996,
4.26678755349596));
#32555=CARTESIAN_POINT('Ctrl Pts',(18.4856613288592,-0.247715549624222,
4.26678755349611));
#32556=CARTESIAN_POINT('Ctrl Pts',(18.4856957875747,-0.247865229791915,
4.26678755349611));
#32557=CARTESIAN_POINT('Ctrl Pts',(18.4857302630303,-0.248014904556736,
4.26678755349611));
#32558=CARTESIAN_POINT('Ctrl Pts',(18.4857647552007,-0.248164573924098,
4.26678755349611));
#32559=CARTESIAN_POINT('Ctrl Pts',(18.5043314682965,-0.32872976226667,4.26678755349766));
#32560=CARTESIAN_POINT('Ctrl Pts',(18.5277911787412,-0.407964970138364,
4.2667875534948));
#32561=CARTESIAN_POINT('Ctrl Pts',(18.552314823445,-0.486910969870589,4.26678755349595));
#32562=CARTESIAN_POINT('Ctrl Pts',(18.552357345021,-0.487047854430916,4.26678755349595));
#32563=CARTESIAN_POINT('Ctrl Pts',(18.55239986991,-0.487184738089763,4.26678755349595));
#32564=CARTESIAN_POINT('Ctrl Pts',(18.5524423981078,-0.487321620848336,
4.26678755349595));
#32565=CARTESIAN_POINT('Ctrl Pts',(18.6015459292246,-0.645367979461387,
4.26678755349831));
#32566=CARTESIAN_POINT('Ctrl Pts',(18.655043587707,-0.802219259702535,4.2667875534954));
#32567=CARTESIAN_POINT('Ctrl Pts',(18.7060174878535,-0.959758075388361,
4.26678755349545));
#32568=CARTESIAN_POINT('Ctrl Pts',(18.7060553290986,-0.959875026708893,
4.26678755349545));
#32569=CARTESIAN_POINT('Ctrl Pts',(18.7060931692692,-0.959991978323139,
4.26678755349545));
#32570=CARTESIAN_POINT('Ctrl Pts',(18.7061310083643,-0.960108930231384,
4.26678755349545));
#32571=CARTESIAN_POINT('Ctrl Pts',(18.8081234684985,-1.27534408100678,4.26678755349557));
#32572=CARTESIAN_POINT('Ctrl Pts',(18.9022854709063,-1.59271847963817,4.26678755349544));
#32573=CARTESIAN_POINT('Ctrl Pts',(18.9681979440421,-1.91781921667449,4.26678755349543));
#32574=CARTESIAN_POINT('Ctrl Pts',(18.9682142463112,-1.91789962451603,4.26678755349543));
#32575=CARTESIAN_POINT('Ctrl Pts',(18.968230546818,-1.91798003264918,4.26678755349543));
#32576=CARTESIAN_POINT('Ctrl Pts',(18.9682468455622,-1.91806044107386,4.26678755349543));
#32577=CARTESIAN_POINT('Ctrl Pts',(19.0011918379723,-2.08059167162913,4.26678755349543));
#32578=CARTESIAN_POINT('Ctrl Pts',(19.0269345328965,-2.24431257125727,4.26678755349543));
#32579=CARTESIAN_POINT('Ctrl Pts',(19.0420990825219,-2.40836704229758,4.26678755349543));
#32580=CARTESIAN_POINT('Ctrl Pts',(19.0572711744983,-2.57250310866618,4.26678755349543));
#32581=CARTESIAN_POINT('Ctrl Pts',(19.0621241707402,-2.73728491562089,4.26678755349543));
#32582=CARTESIAN_POINT('Ctrl Pts',(19.0510253633269,-2.90306553275185,4.26678755349543));
#32583=CARTESIAN_POINT('Ctrl Pts',(19.0510226192503,-2.90310652046414,4.26678755349543));
#32584=CARTESIAN_POINT('Ctrl Pts',(19.0510198741666,-2.90314750825434,4.26678755349543));
#32585=CARTESIAN_POINT('Ctrl Pts',(19.0510171280758,-2.9031884961222,4.26678755349543));
#32586=CARTESIAN_POINT('Ctrl Pts',(19.0454664098095,-2.98603794451841,4.26678755349543));
#32587=CARTESIAN_POINT('Ctrl Pts',(19.0358009037468,-3.06920490198507,4.26678755349543));
#32588=CARTESIAN_POINT('Ctrl Pts',(19.0211988493128,-3.15074112916623,4.26678755349543));
#32589=CARTESIAN_POINT('Ctrl Pts',(19.006589543518,-3.23231784712912,4.26678755349543));
#32590=CARTESIAN_POINT('Ctrl Pts',(18.9870649540648,-3.31269840555977,4.26678755349543));
#32591=CARTESIAN_POINT('Ctrl Pts',(18.9610497328516,-3.39149913067213,4.26678755349543));
#32592=CARTESIAN_POINT('Ctrl Pts',(18.9610433008161,-3.39151861346081,4.26678755349543));
#32593=CARTESIAN_POINT('Ctrl Pts',(18.9610368683589,-3.39153809619381,4.26678755349543));
#32594=CARTESIAN_POINT('Ctrl Pts',(18.9610304354799,-3.39155757887106,4.26678755349543));
#32595=CARTESIAN_POINT('Ctrl Pts',(18.9350182596588,-3.47033829694986,4.26678755349543));
#32596=CARTESIAN_POINT('Ctrl Pts',(18.9021092263951,-3.54820850188026,4.26678755349543));
#32597=CARTESIAN_POINT('Ctrl Pts',(18.8615965006036,-3.62042627660495,4.26678755349543));
#32598=CARTESIAN_POINT('Ctrl Pts',(18.861591491163,-3.62043520640779,4.26678755349543));
#32599=CARTESIAN_POINT('Ctrl Pts',(18.8615864816075,-3.6204441361364,4.26678755349543));
#32600=CARTESIAN_POINT('Ctrl Pts',(18.8615814719371,-3.62045306579077,4.26678755349543));
#32601=CARTESIAN_POINT('Ctrl Pts',(18.8293282449153,-3.67794390791935,4.26678755349543));
#32602=CARTESIAN_POINT('Ctrl Pts',(18.7923266345213,-3.73234026194883,4.26678755349543));
#32603=CARTESIAN_POINT('Ctrl Pts',(18.7484881342047,-3.78228112582125,4.26678755349543));
#32604=CARTESIAN_POINT('Ctrl Pts',(18.7372525105736,-3.79508075961879,4.26678755349543));
#32605=CARTESIAN_POINT('Ctrl Pts',(18.7255675768418,-3.8075875837349,4.26678755349543));
#32606=CARTESIAN_POINT('Ctrl Pts',(18.7133976597241,-3.81977834524697,4.26678755349543));
#32607=CARTESIAN_POINT('Origin',(14.8870768733179,0.,4.26678755349543));
#32608=CARTESIAN_POINT('Origin',(18.3575990203927,-10.,-4.26678755349543));
#32609=CARTESIAN_POINT('',(18.3843475112712,-4.12317055822481,-4.26678755349543));
#32610=CARTESIAN_POINT('Ctrl Pts',(18.3575990203927,-3.99420842564088,-4.26678755349543));
#32611=CARTESIAN_POINT('Ctrl Pts',(18.3575990203927,-4.03574406331344,-4.26678755349543));
#32612=CARTESIAN_POINT('Ctrl Pts',(18.3672627745756,-4.08260100655593,-4.26678755349543));
#32613=CARTESIAN_POINT('Ctrl Pts',(18.3843475112712,-4.1231705582248,-4.26678755349543));
#32614=CARTESIAN_POINT('',(18.7133976597241,-3.81977834524697,-4.26678755349543));
#32615=CARTESIAN_POINT('Origin',(14.8870768733179,0.,-4.26678755349543));
#32616=CARTESIAN_POINT('',(18.4538614420533,0.,-4.26678755349543));
#32617=CARTESIAN_POINT('Ctrl Pts',(18.7133976597241,-3.81977834524697,-4.26678755349543));
#32618=CARTESIAN_POINT('Ctrl Pts',(18.7608818058108,-3.77221286924961,-4.26678755349543));
#32619=CARTESIAN_POINT('Ctrl Pts',(18.8009866046437,-3.71983834098458,-4.26678755349543));
#32620=CARTESIAN_POINT('Ctrl Pts',(18.8358117274585,-3.66402313169491,-4.26678755349543));
#32621=CARTESIAN_POINT('Ctrl Pts',(18.8447418174152,-3.64971062395264,-4.26678755349543));
#32622=CARTESIAN_POINT('Ctrl Pts',(18.8533245106631,-3.63517172105021,-4.26678755349543));
#32623=CARTESIAN_POINT('Ctrl Pts',(18.8615948019429,-3.62042922728382,-4.26678755349543));
#32624=CARTESIAN_POINT('Ctrl Pts',(18.8615953571645,-3.62042823755431,-4.26678755349543));
#32625=CARTESIAN_POINT('Ctrl Pts',(18.8615959123847,-3.6204272478239,-4.26678755349543));
#32626=CARTESIAN_POINT('Ctrl Pts',(18.8615964676035,-3.62042625809258,-4.26678755349543));
#32627=CARTESIAN_POINT('Ctrl Pts',(18.9021180702506,-3.54819257345561,-4.26678755349543));
#32628=CARTESIAN_POINT('Ctrl Pts',(18.9350325943709,-3.4703043534866,-4.26678755349543));
#32629=CARTESIAN_POINT('Ctrl Pts',(18.9610475717044,-3.39150560137125,-4.26678755349543));
#32630=CARTESIAN_POINT('Ctrl Pts',(18.9610482846085,-3.39150344200163,-4.26678755349543));
#32631=CARTESIAN_POINT('Ctrl Pts',(18.9610489975074,-3.39150128263133,-4.26678755349543));
#32632=CARTESIAN_POINT('Ctrl Pts',(18.9610497104011,-3.39149912326034,-4.26678755349543));
#32633=CARTESIAN_POINT('Ctrl Pts',(18.9870650252034,-3.3126981536433,-4.26678755349543));
#32634=CARTESIAN_POINT('Ctrl Pts',(19.0065895569739,-3.23231768034818,-4.26678755349543));
#32635=CARTESIAN_POINT('Ctrl Pts',(19.0211988282645,-3.15074112539677,-4.26678755349543));
#32636=CARTESIAN_POINT('Ctrl Pts',(19.0358072958342,-3.06916905833388,-4.26678755349543));
#32637=CARTESIAN_POINT('Ctrl Pts',(19.0454748719371,-2.98596489662045,-4.26678755349543));
#32638=CARTESIAN_POINT('Ctrl Pts',(19.0510244255707,-2.90307915963347,-4.26678755349543));
#32639=CARTESIAN_POINT('Ctrl Pts',(19.0510247297345,-2.90307461677399,-4.26678755349543));
#32640=CARTESIAN_POINT('Ctrl Pts',(19.0510250338859,-2.90307007391548,-4.26678755349543));
#32641=CARTESIAN_POINT('Ctrl Pts',(19.051025338025,-2.90306553105792,-4.26678755349543));
#32642=CARTESIAN_POINT('Ctrl Pts',(19.062124153563,-2.73728499936675,-4.26678755349543));
#32643=CARTESIAN_POINT('Ctrl Pts',(19.0572711633294,-2.57250305359533,-4.26678755349543));
#32644=CARTESIAN_POINT('Ctrl Pts',(19.0420990719329,-2.40836704327638,-4.26678755349543));
#32645=CARTESIAN_POINT('Ctrl Pts',(19.0269278165402,-2.24424007708595,-4.26678755349543));
#32646=CARTESIAN_POINT('Ctrl Pts',(19.0011690644904,-2.08044717424057,-4.26678755349543));
#32647=CARTESIAN_POINT('Ctrl Pts',(18.9682033134569,-1.91784596289597,-4.26678755349543));
#32648=CARTESIAN_POINT('Ctrl Pts',(18.9682015066474,-1.91783705093721,-4.26678755349543));
#32649=CARTESIAN_POINT('Ctrl Pts',(18.9681996998163,-1.91782813898203,-4.26678755349543));
#32650=CARTESIAN_POINT('Ctrl Pts',(18.9681978929635,-1.91781922703043,-4.26678755349543));
#32651=CARTESIAN_POINT('Ctrl Pts',(18.9022638977272,-1.59261256156863,-4.26678755349543));
#32652=CARTESIAN_POINT('Ctrl Pts',(18.8080608958824,-1.27513481155645,-4.26678755349543));
#32653=CARTESIAN_POINT('Ctrl Pts',(18.7060299372189,-0.959797005169111,
-4.26678755349543));
#32654=CARTESIAN_POINT('Ctrl Pts',(18.7060257431389,-0.959784042907454,
-4.26678755349543));
#32655=CARTESIAN_POINT('Ctrl Pts',(18.7060215490457,-0.95977108064926,-4.26678755349543));
#32656=CARTESIAN_POINT('Ctrl Pts',(18.7060173549391,-0.959758118394527,
-4.26678755349543));
#32657=CARTESIAN_POINT('Ctrl Pts',(18.6550043488165,-0.802097940920412,
-4.26678755349543));
#32658=CARTESIAN_POINT('Ctrl Pts',(18.6014547932599,-0.64510416345673,-4.26678755349549));
#32659=CARTESIAN_POINT('Ctrl Pts',(18.5523323438895,-0.486969437517935,
-4.26678755349544));
#32660=CARTESIAN_POINT('Ctrl Pts',(18.5523263086478,-0.486950008900037,
-4.26678755349544));
#32661=CARTESIAN_POINT('Ctrl Pts',(18.552320273473,-0.486930580264954,-4.26678755349544));
#32662=CARTESIAN_POINT('Ctrl Pts',(18.552314238365,-0.486911151612686,-4.26678755349544));
#32663=CARTESIAN_POINT('Ctrl Pts',(18.5277575741225,-0.40785657677535,-4.26678755349541));
#32664=CARTESIAN_POINT('Ctrl Pts',(18.5042740984017,-0.328527131581695,
-4.266787553496));
#32665=CARTESIAN_POINT('Ctrl Pts',(18.4857119715276,-0.247937289204806,
-4.2667875534956));
#32666=CARTESIAN_POINT('Ctrl Pts',(18.4856949543482,-0.247863406948809,
-4.2667875534956));
#32667=CARTESIAN_POINT('Ctrl Pts',(18.4856779414224,-0.247789524151342,
-4.2667875534956));
#32668=CARTESIAN_POINT('Ctrl Pts',(18.4856609327526,-0.247715640809645,
-4.2667875534956));
#32669=CARTESIAN_POINT('Ctrl Pts',(18.4781251595079,-0.214981269683404,
-4.26678755349544));
#32670=CARTESIAN_POINT('Ctrl Pts',(18.4714946508473,-0.182018340757567,
-4.26678755349544));
#32671=CARTESIAN_POINT('Ctrl Pts',(18.4662508311777,-0.148698263420427,
-4.26678755349543));
#32672=CARTESIAN_POINT('Ctrl Pts',(18.4619453320882,-0.121340426637857,
-4.26678755349543));
#32673=CARTESIAN_POINT('Ctrl Pts',(18.4585740060291,-0.0937414373303757,
-4.26678755349543));
#32674=CARTESIAN_POINT('Ctrl Pts',(18.4564380870412,-0.0658241261208444,
-4.26678755349543));
#32675=CARTESIAN_POINT('Ctrl Pts',(18.4547751193048,-0.0440884759903845,
-4.26678755349543));
#32676=CARTESIAN_POINT('Ctrl Pts',(18.4538614420616,-0.0221597443920782,
-4.26678755349543));
#32677=CARTESIAN_POINT('Ctrl Pts',(18.4538614420644,-2.56805687826045E-12,
-4.26678755349543));
#32678=CARTESIAN_POINT('',(18.3575990203927,0.,-4.26678755349543));
#32679=CARTESIAN_POINT('Origin',(14.8870768733179,0.,0.));
#32680=CARTESIAN_POINT('Origin',(18.4538614420533,1.29836352043984E-18,
-4.76678755349543));
#32681=CARTESIAN_POINT('Origin',(14.8870768733179,0.,0.));
#32682=CARTESIAN_POINT('Origin',(18.4538614420533,3.76800988090885E-16,
4.76678755349543));
#32683=CARTESIAN_POINT('Ctrl Pts',(18.6542359870042,-4.26970425052901,-5.14005510487642));
#32684=CARTESIAN_POINT('Ctrl Pts',(19.0577899084937,-5.18691783079565,-4.26678755349586));
#32685=CARTESIAN_POINT('Ctrl Pts',(18.5204132448321,-3.96090161554629,-4.26678755349543));
#32686=CARTESIAN_POINT('Ctrl Pts',(18.9222117185918,-4.16007568622317,-5.11560140424043));
#32687=CARTESIAN_POINT('Ctrl Pts',(19.4799272843404,-4.78635337341915,-4.26678755349528));
#32688=CARTESIAN_POINT('Ctrl Pts',(18.6801136214415,-3.87779830058524,-4.26678755349543));
#32689=CARTESIAN_POINT('Ctrl Pts',(19.0979593370657,-4.00248991871804,-5.07972521647459));
#32690=CARTESIAN_POINT('Ctrl Pts',(19.6110505295027,-4.40503233983348,-4.26678755349543));
#32691=CARTESIAN_POINT('Ctrl Pts',(18.7844712393506,-3.75790943902247,-4.26678755349543));
#32692=CARTESIAN_POINT('Ctrl Pts',(19.2959765085615,-3.73301197651848,-5.01655082533848));
#32693=CARTESIAN_POINT('Ctrl Pts',(19.68659106153,-3.91712710693031,-4.26678755349543));
#32694=CARTESIAN_POINT('Ctrl Pts',(18.9021191809457,-3.54819059360291,-4.26678755349543));
#32695=CARTESIAN_POINT('Ctrl Pts',(19.3513956440603,-3.63388752247013,-4.99301158143074));
#32696=CARTESIAN_POINT('Ctrl Pts',(19.6930611405989,-3.7699368058973,-4.26678755349543));
#32697=CARTESIAN_POINT('Ctrl Pts',(18.9350343692454,-3.47030011905697,-4.26678755349543));
#32698=CARTESIAN_POINT('Ctrl Pts',(19.4390223899416,-3.43576678210827,-4.94534871538099));
#32699=CARTESIAN_POINT('Ctrl Pts',(19.6880690365751,-3.50527002686798,-4.26678755349543));
#32700=CARTESIAN_POINT('Ctrl Pts',(18.9870650305019,-3.31269812051263,-4.26678755349543));
#32701=CARTESIAN_POINT('Ctrl Pts',(19.4719166463349,-3.33589127417514,-4.92102514232829));
#32702=CARTESIAN_POINT('Ctrl Pts',(19.6779161308525,-3.38370254509204,-4.26678755349543));
#32703=CARTESIAN_POINT('Ctrl Pts',(19.0065895537831,-3.23231765789036,-4.26678755349543));
#32704=CARTESIAN_POINT('Ctrl Pts',(19.5211651350852,-3.13583705072043,-4.87181032321129));
#32705=CARTESIAN_POINT('Ctrl Pts',(19.6488720310131,-3.15520989470188,-4.26678755349543));
#32706=CARTESIAN_POINT('Ctrl Pts',(19.0358080846578,-3.06916458966381,-4.26678755349543));
#32707=CARTESIAN_POINT('Ctrl Pts',(19.5374740961704,-3.03514253616215,-4.84678973600571));
#32708=CARTESIAN_POINT('Ctrl Pts',(19.6302244752384,-3.04627737812982,-4.26678755349543));
#32709=CARTESIAN_POINT('Ctrl Pts',(19.0454759169275,-2.98595579110855,-4.26678755349543));
#32710=CARTESIAN_POINT('Ctrl Pts',(19.5656064151764,-2.73847376165093,-4.77259844285197));
#32711=CARTESIAN_POINT('Ctrl Pts',(19.5684120549786,-2.74532693995999,-4.26678755349543));
#32712=CARTESIAN_POINT('Ctrl Pts',(19.0621241480217,-2.73728500880102,-4.26678755349543));
#32713=CARTESIAN_POINT('Ctrl Pts',(19.557505688877,-2.54754173168078,-4.72420514209177));
#32714=CARTESIAN_POINT('Ctrl Pts',(19.5170237058281,-2.55560043450117,-4.26678755349543));
#32715=CARTESIAN_POINT('Ctrl Pts',(19.057271160227,-2.57250304610011,-4.26678755349543));
#32716=CARTESIAN_POINT('Ctrl Pts',(19.5065540718371,-2.17859460722192,-4.63142824827105));
#32717=CARTESIAN_POINT('Ctrl Pts',(19.4034908984912,-2.19830057322816,-4.26678755349543));
#32718=CARTESIAN_POINT('Ctrl Pts',(19.0269269806048,-2.2442310407331,-4.26678755349543));
#32719=CARTESIAN_POINT('Ctrl Pts',(19.463245787281,-2.00027050534638,-4.58697424177898));
#32720=CARTESIAN_POINT('Ctrl Pts',(19.3409663838283,-2.02616314418212,-4.26678755349543));
#32721=CARTESIAN_POINT('Ctrl Pts',(19.0011662279257,-2.08042916291789,-4.26678755349543));
#32722=CARTESIAN_POINT('Ctrl Pts',(19.2968891634531,-1.48548484252353,-4.46363148732574));
#32723=CARTESIAN_POINT('Ctrl Pts',(19.1483011492445,-1.54320588831284,-4.26678755349543));
#32724=CARTESIAN_POINT('Ctrl Pts',(18.9022612159307,-1.59259935669665,-4.26678755349543));
#32725=CARTESIAN_POINT('Ctrl Pts',(19.1383625511518,-1.17253950176775,-4.39559658478723));
#32726=CARTESIAN_POINT('Ctrl Pts',(18.9990590372986,-1.2248828326142,-4.26678755349543));
#32727=CARTESIAN_POINT('Ctrl Pts',(18.8080530853766,-1.27510872906601,-4.26678755349543));
#32728=CARTESIAN_POINT('Ctrl Pts',(18.8807693660449,-0.726865400089183,
-4.32494765329133));
#32729=CARTESIAN_POINT('Ctrl Pts',(18.7752223218753,-0.764223859480729,
-4.26678755349543));
#32730=CARTESIAN_POINT('Ctrl Pts',(18.6549994601397,-0.802082822630004,
-4.26678755349543));
#32731=CARTESIAN_POINT('Ctrl Pts',(18.7906375006256,-0.582332400014721,
-4.30661231556638));
#32732=CARTESIAN_POINT('Ctrl Pts',(18.70016617769,-0.613489035379009,-4.26678755349543));
#32733=CARTESIAN_POINT('Ctrl Pts',(18.6014509972619,-0.645096921999166,
-4.26678755349543));
#32734=CARTESIAN_POINT('Ctrl Pts',(18.6665728209963,-0.366692065764295,
-4.28782126317335));
#32735=CARTESIAN_POINT('Ctrl Pts',(18.5987003778136,-0.387079548706928,
-4.26678755349543));
#32736=CARTESIAN_POINT('Ctrl Pts',(18.5277457016063,-0.407818315284394,
-4.26678755349543));
#32737=CARTESIAN_POINT('Ctrl Pts',(18.6270102662637,-0.295011052175803,
-4.28300214458113));
#32738=CARTESIAN_POINT('Ctrl Pts',(18.5666581019247,-0.31158967965086,-4.26678755349536));
#32739=CARTESIAN_POINT('Ctrl Pts',(18.5042426057229,-0.328435858715435,
-4.26678755349543));
#32740=CARTESIAN_POINT('Ctrl Pts',(18.5361976874514,-0.0841343764222963,
-4.27345035595134));
#32741=CARTESIAN_POINT('Ctrl Pts',(18.4936062418503,-0.0895865205474039,
-4.26678755349556));
#32742=CARTESIAN_POINT('Ctrl Pts',(18.4502940130769,-0.0940844251823421,
-4.26678755349543));
#32743=CARTESIAN_POINT('Ctrl Pts',(18.5093786690843,0.0599803308146132,
-4.27270022961939));
#32744=CARTESIAN_POINT('Ctrl Pts',(18.4720206072776,0.0639366199169896,
-4.26678755349649));
#32745=CARTESIAN_POINT('Ctrl Pts',(18.4343618285263,0.0671004789595955,
-4.26678755349543));
#32746=CARTESIAN_POINT('Ctrl Pts',(18.6063997166192,0.207276912386747,-4.27916424911031));
#32747=CARTESIAN_POINT('Ctrl Pts',(18.5500685617386,0.219135615093589,-4.26678755349219));
#32748=CARTESIAN_POINT('Ctrl Pts',(18.4919985205465,0.231010279447602,-4.26678755349543));
#32749=CARTESIAN_POINT('Origin',(18.7133976597241,-3.81977834524697,-4.76678755349543));
#32750=CARTESIAN_POINT('Origin',(14.8870768733179,0.,-4.76678755349543));
#32751=CARTESIAN_POINT('Ctrl Pts',(18.7837086993174,-4.27128032554705,-5.09745204146194));
#32752=CARTESIAN_POINT('Ctrl Pts',(18.7837837624154,-4.27218856939587,-5.09663362133658));
#32753=CARTESIAN_POINT('Ctrl Pts',(18.7838569011206,-4.27309483878909,-5.0958128351685));
#32754=CARTESIAN_POINT('Ctrl Pts',(18.787810353939,-4.32329670754872,-5.05011558445576));
#32755=CARTESIAN_POINT('Ctrl Pts',(18.7859513395349,-4.36654052586954,-4.99838378394199));
#32756=CARTESIAN_POINT('Ctrl Pts',(18.7708050164925,-4.43566404078374,-4.88679567157663));
#32757=CARTESIAN_POINT('Ctrl Pts',(18.7578033695063,-4.46162539414925,-4.82752476395243));
#32758=CARTESIAN_POINT('Ctrl Pts',(18.7204855200627,-4.49373583225153,-4.70302915637018));
#32759=CARTESIAN_POINT('Ctrl Pts',(18.6958976213804,-4.49858998809844,-4.63853166786264));
#32760=CARTESIAN_POINT('Ctrl Pts',(18.6406738757079,-4.48244009347221,-4.52164441884446));
#32761=CARTESIAN_POINT('Ctrl Pts',(18.6114407022608,-4.46403154155928,-4.46994402103078));
#32762=CARTESIAN_POINT('Ctrl Pts',(18.5512951506147,-4.40736654541262,-4.38235276133824));
#32763=CARTESIAN_POINT('Ctrl Pts',(18.5214085776067,-4.37097137724525,-4.34705233647852));
#32764=CARTESIAN_POINT('Ctrl Pts',(18.4626511753395,-4.28318578164407,-4.29387508247684));
#32765=CARTESIAN_POINT('Ctrl Pts',(18.4346965748636,-4.2329044689914,-4.27709516144855));
#32766=CARTESIAN_POINT('Ctrl Pts',(18.4006544833022,-4.16080775958966,-4.26793451055797));
#32767=CARTESIAN_POINT('Ctrl Pts',(18.3923049583211,-4.14206637529222,-4.26678755349543));
#32768=CARTESIAN_POINT('Ctrl Pts',(18.3843475112712,-4.1231705582248,-4.26678755349543));
#32769=CARTESIAN_POINT('Origin',(14.8870768733179,-3.99420842564088,0.));
#32770=CARTESIAN_POINT('Ctrl Pts',(11.1585526803519,-4.38134327770264,-5.09856534401066));
#32771=CARTESIAN_POINT('Ctrl Pts',(11.1773095544415,-4.40043210711516,-5.08334924385387));
#32772=CARTESIAN_POINT('Ctrl Pts',(11.1965634146953,-4.41737314983265,-5.0663896003135));
#32773=CARTESIAN_POINT('Ctrl Pts',(11.2160327360732,-4.43193019040154,-5.04794583054052));
#32774=CARTESIAN_POINT('Ctrl Pts',(11.235499063637,-4.44648499252185,-5.02950489688177));
#32775=CARTESIAN_POINT('Ctrl Pts',(11.2551808637128,-4.45865655224405,-5.0095803001658));
#32776=CARTESIAN_POINT('Ctrl Pts',(11.2747924288633,-4.46825273215176,-4.98845874515855));
#32777=CARTESIAN_POINT('Ctrl Pts',(11.2941553527337,-4.47772724882462,-4.9676049755338));
#32778=CARTESIAN_POINT('Ctrl Pts',(11.3134499541213,-4.48469120824842,-4.94558445055882));
#32779=CARTESIAN_POINT('Ctrl Pts',(11.3323953866326,-4.48900270879227,-4.9226994094508));
#32780=CARTESIAN_POINT('Ctrl Pts',(11.3351876321147,-4.48963815313524,-4.91932653038861));
#32781=CARTESIAN_POINT('Ctrl Pts',(11.3379722800483,-4.4902160597842,-4.91593491878871));
#32782=CARTESIAN_POINT('Ctrl Pts',(11.3407484170919,-4.49073605743578,-4.91252559036193));
#32783=CARTESIAN_POINT('Ctrl Pts',(11.3547633161217,-4.49336118525482,-4.89531412244419));
#32784=CARTESIAN_POINT('Ctrl Pts',(11.3685552099567,-4.49450846568627,-4.87762256908707));
#32785=CARTESIAN_POINT('Ctrl Pts',(11.3819878602132,-4.49414152262891,-4.85965719763253));
#32786=CARTESIAN_POINT('Ctrl Pts',(11.3954056409517,-4.49377498576589,-4.84171171327456));
#32787=CARTESIAN_POINT('Ctrl Pts',(11.4084645659427,-4.49189752730234,-4.82349370723202));
#32788=CARTESIAN_POINT('Ctrl Pts',(11.4210277728046,-4.48852481095031,-4.80521097378418));
#32789=CARTESIAN_POINT('Ctrl Pts',(11.433582228137,-4.48515444403239,-4.78694097608782));
#32790=CARTESIAN_POINT('Ctrl Pts',(11.4456412560894,-4.48029104788819,-4.76860702043759));
#32791=CARTESIAN_POINT('Ctrl Pts',(11.4570732740616,-4.47400139883439,-4.75040836654757));
#32792=CARTESIAN_POINT('Ctrl Pts',(11.468515105606,-4.46770635056538,-4.73219409041087));
#32793=CARTESIAN_POINT('Ctrl Pts',(11.4793284781849,-4.4599829216249,-4.71411597746034));
#32794=CARTESIAN_POINT('Ctrl Pts',(11.4893922899614,-4.45094580241366,-4.69635581925028));
#32795=CARTESIAN_POINT('Ctrl Pts',(11.492098904207,-4.44851531224363,-4.69157930928745));
#32796=CARTESIAN_POINT('Ctrl Pts',(11.4947513791465,-4.44599005094159,-4.68682566810472));
#32797=CARTESIAN_POINT('Ctrl Pts',(11.4973475437834,-4.44337278306917,-4.68209812382677));
#32798=CARTESIAN_POINT('Ctrl Pts',(11.5077296350375,-4.43290629974145,-4.66319262168548));
#32799=CARTESIAN_POINT('Ctrl Pts',(11.5172734125901,-4.42090574709506,-4.64460238394084));
#32800=CARTESIAN_POINT('Ctrl Pts',(11.5258955869577,-4.407513147548,-4.62655201641156));
#32801=CARTESIAN_POINT('Ctrl Pts',(11.5345249584581,-4.39410936888171,-4.60848658181409));
#32802=CARTESIAN_POINT('Ctrl Pts',(11.542230869974,-4.37931167764791,-4.59096238287243));
#32803=CARTESIAN_POINT('Ctrl Pts',(11.5489433162915,-4.36330323603274,-4.57417465116145));
#32804=CARTESIAN_POINT('Ctrl Pts',(11.5556857006915,-4.34722339540373,-4.55731204473639));
#32805=CARTESIAN_POINT('Ctrl Pts',(11.5614254453184,-4.32992254541936,-4.54119286157343));
#32806=CARTESIAN_POINT('Ctrl Pts',(11.5661098411331,-4.31161973967097,-4.52597841654605));
#32807=CARTESIAN_POINT('Ctrl Pts',(11.5705971850957,-4.29408685216031,-4.51140397605482));
#32808=CARTESIAN_POINT('Ctrl Pts',(11.5741160472694,-4.27563526415019,-4.49765968024976));
#32809=CARTESIAN_POINT('Ctrl Pts',(11.5766390463655,-4.25647826147464,-4.48485227017963));
#32810=CARTESIAN_POINT('Ctrl Pts',(11.5794931650594,-4.23480708468317,-4.47036400953826));
#32811=CARTESIAN_POINT('Ctrl Pts',(11.5810960704834,-4.21214692058059,-4.45702539669295));
#32812=CARTESIAN_POINT('Ctrl Pts',(11.5814513272679,-4.18878092056111,-4.44498843496028));
#32813=CARTESIAN_POINT('Ctrl Pts',(11.5818079107881,-4.1653276582881,-4.4329065202016));
#32814=CARTESIAN_POINT('Ctrl Pts',(11.5809072717996,-4.14116392284387,-4.42213601636339));
#32815=CARTESIAN_POINT('Ctrl Pts',(11.5787776008217,-4.11659012936366,-4.41278615285239));
#32816=CARTESIAN_POINT('Ctrl Pts',(11.5766350578908,-4.09186780931835,-4.40337977779331));
#32817=CARTESIAN_POINT('Ctrl Pts',(11.5732483837194,-4.06673113284847,-4.39541118322439));
#32818=CARTESIAN_POINT('Ctrl Pts',(11.5686744386717,-4.04149025072602,-4.388947118107));
#32819=CARTESIAN_POINT('Ctrl Pts',(11.5658212792752,-4.02574536108437,-4.38491492971454));
#32820=CARTESIAN_POINT('Ctrl Pts',(11.5625067173491,-4.0099599694054,-4.38146728159009));
#32821=CARTESIAN_POINT('Ctrl Pts',(11.5587504889214,-3.99420842564088,-4.37861204937474));
#32822=CARTESIAN_POINT('Ctrl Pts',(11.6023844202601,-3.95458824321301,-4.41143916299716));
#32823=CARTESIAN_POINT('Ctrl Pts',(12.0832028940249,-4.85453203063264,-4.76944949788135));
#32824=CARTESIAN_POINT('Ctrl Pts',(11.2797574433457,-4.27163583400664,-5.19835981118057));
#32825=CARTESIAN_POINT('Ctrl Pts',(11.2965510773294,-4.23166746059414,-4.18372017236837));
#32826=CARTESIAN_POINT('Ctrl Pts',(11.7265205257192,-5.02989742734166,-4.55166507795904));
#32827=CARTESIAN_POINT('Ctrl Pts',(10.9461377790192,-4.57173371007227,-4.93102752573452));
#32828=CARTESIAN_POINT('Ctrl Pts',(11.0041813520405,-4.50935327267487,-3.91588406330021));
#32829=CARTESIAN_POINT('Ctrl Pts',(11.35463790312,-5.24827427945486,-4.26941570590351));
#32830=CARTESIAN_POINT('Ctrl Pts',(10.6271700716899,-4.8726684807913,-4.61619738710776));
#32831=CARTESIAN_POINT('Ctrl Pts',(10.4769208212593,-5.01960677357028,-3.31082304312022));
#32832=CARTESIAN_POINT('Ctrl Pts',(10.7063724913704,-5.66598932993541,-3.61715501248506));
#32833=CARTESIAN_POINT('Ctrl Pts',(10.0519760808134,-5.42585676036716,-3.90424156632786));
#32834=CARTESIAN_POINT('Ctrl Pts',(10.2416197998638,-5.25263344048483,-2.97536444930372));
#32835=CARTESIAN_POINT('Ctrl Pts',(10.4143336358881,-5.8700643207334,-3.25312151833443));
#32836=CARTESIAN_POINT('Ctrl Pts',(9.79528424049654,-5.67861782892684,-3.50918796214299));
#32837=CARTESIAN_POINT('Ctrl Pts',(9.93843086546135,-5.55540857377054,-2.40970308249717));
#32838=CARTESIAN_POINT('Ctrl Pts',(10.0432225556495,-6.13934804787589,-2.62610418078175));
#32839=CARTESIAN_POINT('Ctrl Pts',(9.46453287938951,-6.00714081830833,-2.8425598401767));
#32840=CARTESIAN_POINT('Ctrl Pts',(9.84630047984833,-5.64795878660729,-2.2110461725345));
#32841=CARTESIAN_POINT('Ctrl Pts',(9.93245569216299,-6.22144594389688,-2.40973271653319));
#32842=CARTESIAN_POINT('Ctrl Pts',(9.36402698495814,-6.10758192572937,-2.60837180214158));
#32843=CARTESIAN_POINT('Ctrl Pts',(9.68617352369147,-5.80932527533534,-1.80243062942356));
#32844=CARTESIAN_POINT('Ctrl Pts',(9.74203346991433,-6.36432738273618,-1.96549235930559));
#32845=CARTESIAN_POINT('Ctrl Pts',(9.18934290808578,-6.28272973353952,-2.1265495309748));
#32846=CARTESIAN_POINT('Ctrl Pts',(9.61741694726934,-5.8789033577973,-1.59116370555004));
#32847=CARTESIAN_POINT('Ctrl Pts',(9.65983154833276,-6.42693601101231,-1.73484105847517));
#32848=CARTESIAN_POINT('Ctrl Pts',(9.11433573142727,-6.35826284245593,-1.87737372989252));
#32849=CARTESIAN_POINT('Ctrl Pts',(9.50459929783986,-5.99327376404412,-1.15327916114787));
#32850=CARTESIAN_POINT('Ctrl Pts',(9.52636981824612,-6.52928853743275,-1.25828708926425));
#32851=CARTESIAN_POINT('Ctrl Pts',(8.99126185288356,-6.48243255916743,-1.36082662439774));
#32852=CARTESIAN_POINT('Ctrl Pts',(9.4604583322397,-6.03814934571557,-0.924683260137496));
#32853=CARTESIAN_POINT('Ctrl Pts',(9.47377323241263,-6.57003899685759,-1.00827566940964));
#32854=CARTESIAN_POINT('Ctrl Pts',(8.94310807720623,-6.53115944545418,-1.0911207364409));
#32855=CARTESIAN_POINT('Ctrl Pts',(9.40208193744606,-6.09753305073092,-0.466967317285123));
#32856=CARTESIAN_POINT('Ctrl Pts',(9.40492964574317,-6.6235022859682,-0.509879942965713));
#32857=CARTESIAN_POINT('Ctrl Pts',(8.87942469755632,-6.59564165953961,-0.551041961059405));
#32858=CARTESIAN_POINT('Ctrl Pts',(9.3872659867011,-6.1126296856763,-0.236515666537748));
#32859=CARTESIAN_POINT('Ctrl Pts',(9.38729967348299,-6.63727567478022,-0.257585124159667));
#32860=CARTESIAN_POINT('Ctrl Pts',(8.86326184534119,-6.61203578049681,-0.279099068085999));
#32861=CARTESIAN_POINT('Ctrl Pts',(9.38689134318635,-6.11301121950842,0.22763695481613));
#32862=CARTESIAN_POINT('Ctrl Pts',(9.38685830965689,-6.63761983283789,0.247898500448822));
#32863=CARTESIAN_POINT('Ctrl Pts',(8.86285314380986,-6.61245009557666,0.268621792442221));
#32864=CARTESIAN_POINT('Ctrl Pts',(9.40176342855522,-6.09785739024047,0.463304811352815));
#32865=CARTESIAN_POINT('Ctrl Pts',(9.40455284931414,-6.62379599714687,0.505887165407633));
#32866=CARTESIAN_POINT('Ctrl Pts',(8.87907723400249,-6.59599386455161,0.546720178855904));
#32867=CARTESIAN_POINT('Ctrl Pts',(9.4598972513562,-6.03871977872338,0.921431650466073));
#32868=CARTESIAN_POINT('Ctrl Pts',(9.47310966312735,-6.57055322886647,1.00473113009131));
#32869=CARTESIAN_POINT('Ctrl Pts',(8.94249598790001,-6.53177883552457,1.08728425276695));
#32870=CARTESIAN_POINT('Ctrl Pts',(9.50290925766476,-5.99499017867409,1.14539763783599));
#32871=CARTESIAN_POINT('Ctrl Pts',(9.52436700384407,-6.53083458388161,1.24969833999858));
#32872=CARTESIAN_POINT('Ctrl Pts',(8.98941817134168,-6.48429618975125,1.35152822695961));
#32873=CARTESIAN_POINT('Ctrl Pts',(9.61518610363573,-5.88116189868735,1.58378166890141));
#32874=CARTESIAN_POINT('Ctrl Pts',(9.65718258741704,-6.42895757477472,1.72680004328843));
#32875=CARTESIAN_POINT('Ctrl Pts',(9.11190208330511,-6.36071474771872,1.86866655378836));
#32876=CARTESIAN_POINT('Ctrl Pts',(9.68512122038265,-5.81038739427925,1.7995430161374));
#32877=CARTESIAN_POINT('Ctrl Pts',(9.74079777647695,-6.36525992343917,1.96238829694538));
#32878=CARTESIAN_POINT('Ctrl Pts',(9.18819493952837,-6.28388263584057,2.12314424680613));
#32879=CARTESIAN_POINT('Ctrl Pts',(9.84601632803572,-5.64824348202644,2.21052171688795));
#32880=CARTESIAN_POINT('Ctrl Pts',(9.93213061479567,-6.2216843877734,2.40920076822843));
#32881=CARTESIAN_POINT('Ctrl Pts',(9.36371699951435,-6.10789086343246,2.60775370952373));
#32882=CARTESIAN_POINT('Ctrl Pts',(9.9370833975153,-5.55676033002984,2.40689371529671));
#32883=CARTESIAN_POINT('Ctrl Pts',(10.0415975635527,-6.14054654730368,2.62303197976634));
#32884=CARTESIAN_POINT('Ctrl Pts',(9.46306291377357,-6.00860775242521,2.83924822810719));
#32885=CARTESIAN_POINT('Ctrl Pts',(10.1385376408381,-5.35556888418775,2.78333395855106));
#32886=CARTESIAN_POINT('Ctrl Pts',(10.2829804663152,-5.96535627785836,3.03152616052292));
#32887=CARTESIAN_POINT('Ctrl Pts',(9.68283135755879,-5.79030632466165,3.28288272234244));
#32888=CARTESIAN_POINT('Ctrl Pts',(10.2496800262008,-5.24511502447779,2.96433987393686));
#32889=CARTESIAN_POINT('Ctrl Pts',(10.4176330616188,-5.86950598460442,3.22787521677906));
#32890=CARTESIAN_POINT('Ctrl Pts',(9.80407764728161,-5.67047963099968,3.49612647446564));
#32891=CARTESIAN_POINT('Ctrl Pts',(10.4853605723167,-5.01279790466392,3.30418734507658));
#32892=CARTESIAN_POINT('Ctrl Pts',(10.7029082049272,-5.67232521767017,3.59542004999764));
#32893=CARTESIAN_POINT('Ctrl Pts',(10.0611839441483,-5.41850504752442,3.89635328060898));
#32894=CARTESIAN_POINT('Ctrl Pts',(10.6100710485857,-4.89074738772537,3.46366781290886));
#32895=CARTESIAN_POINT('Ctrl Pts',(10.8555706827195,-5.56984011245734,3.76732714942));
#32896=CARTESIAN_POINT('Ctrl Pts',(10.1972318335047,-5.28615378358059,4.08409029398417));
#32897=CARTESIAN_POINT('Ctrl Pts',(11.0032082744194,-4.5103029492058,3.91467225682926));
#32898=CARTESIAN_POINT('Ctrl Pts',(11.3532021212208,-5.24922620608444,4.26785123513628));
#32899=CARTESIAN_POINT('Ctrl Pts',(10.6261085431467,-4.87369823287049,4.61477103735768));
#32900=CARTESIAN_POINT('Ctrl Pts',(11.2905193056397,-4.23711761886764,4.17928334636283));
#32901=CARTESIAN_POINT('Ctrl Pts',(11.7200923343516,-5.03301753809122,4.54780361973909));
#32902=CARTESIAN_POINT('Ctrl Pts',(10.9395311093629,-4.57766067780649,4.92579774106571));
#32903=CARTESIAN_POINT('Ctrl Pts',(11.6028786121923,-3.95414052617678,4.41180708798777));
#32904=CARTESIAN_POINT('Ctrl Pts',(12.0838277141608,-4.85422486814698,4.7698309482503));
#32905=CARTESIAN_POINT('Ctrl Pts',(11.2802965629704,-4.2711508971833,5.1987917615104));
#32906=CARTESIAN_POINT('Origin',(14.8870768733179,0.,4.76678755349543));
#32907=CARTESIAN_POINT('Origin',(18.7133976597241,-3.81977834524697,4.76678755349543));
#32908=CARTESIAN_POINT('Ctrl Pts',(18.3213959387515,-4.03643772855571,4.26678755349542));
#32909=CARTESIAN_POINT('Ctrl Pts',(18.3628668507259,-5.69599427429396,4.26678755349538));
#32910=CARTESIAN_POINT('Ctrl Pts',(18.3206061393696,-4.3689680817557,5.16231907827289));
#32911=CARTESIAN_POINT('Ctrl Pts',(18.6000581110489,-3.96321773775833,4.26678755349543));
#32912=CARTESIAN_POINT('Ctrl Pts',(19.3550672533386,-5.12141477481277,4.26678755349543));
#32913=CARTESIAN_POINT('Ctrl Pts',(18.7871890557531,-4.27257317214253,5.14144467458254));
#32914=CARTESIAN_POINT('Ctrl Pts',(18.7562374053204,-3.80823898150579,4.26678755349543));
#32915=CARTESIAN_POINT('Ctrl Pts',(19.5903948914683,-4.54592068587282,4.26678755349542));
#32916=CARTESIAN_POINT('Ctrl Pts',(19.0502150680539,-4.06694516153942,5.09523814558191));
#32917=CARTESIAN_POINT('Ctrl Pts',(18.9021191809457,-3.54819059360296,4.26678755349543));
#32918=CARTESIAN_POINT('Ctrl Pts',(19.6873927813158,-3.91750415511995,4.26678755349543));
#32919=CARTESIAN_POINT('Ctrl Pts',(19.2957763038374,-3.73291761076936,5.01693471360131));
#32920=CARTESIAN_POINT('Ctrl Pts',(18.9350343692453,-3.47030011905699,4.26678755349543));
#32921=CARTESIAN_POINT('Ctrl Pts',(19.6938018869037,-3.77022961187328,4.26678755349543));
#32922=CARTESIAN_POINT('Ctrl Pts',(19.3512124829545,-3.63381458932239,4.99340047650924));
#32923=CARTESIAN_POINT('Ctrl Pts',(18.9870650305019,-3.31269812051263,4.26678755349543));
#32924=CARTESIAN_POINT('Ctrl Pts',(19.6887012979566,-3.50544371457661,4.26678755349543));
#32925=CARTESIAN_POINT('Ctrl Pts',(19.4388776981255,-3.43572640272002,4.94574244817469));
#32926=CARTESIAN_POINT('Ctrl Pts',(19.0065895537831,-3.23231765789036,4.26678755349543));
#32927=CARTESIAN_POINT('Ctrl Pts',(19.6785000210075,-3.38383421296915,4.26678755349542));
#32928=CARTESIAN_POINT('Ctrl Pts',(19.4717925115843,-3.3358624643861,4.92141882649626));
#32929=CARTESIAN_POINT('Ctrl Pts',(19.0358080846578,-3.06916458966381,4.26678755349543));
#32930=CARTESIAN_POINT('Ctrl Pts',(19.6493709517514,-3.15527991967624,4.26678755349543));
#32931=CARTESIAN_POINT('Ctrl Pts',(19.5210828374545,-3.1358245681776,4.8721994557354));
#32932=CARTESIAN_POINT('Ctrl Pts',(19.0454759169275,-2.98595579110855,4.26678755349543));
#32933=CARTESIAN_POINT('Ctrl Pts',(19.6306860078638,-3.04632498898756,4.26678755349543));
#32934=CARTESIAN_POINT('Ctrl Pts',(19.5374124319044,-3.03513513584574,4.84717438865481));
#32935=CARTESIAN_POINT('Ctrl Pts',(19.0621241480217,-2.737285008801,4.26678755349543));
#32936=CARTESIAN_POINT('Ctrl Pts',(19.5687800824396,-2.74533278574744,4.26678755349543));
#32937=CARTESIAN_POINT('Ctrl Pts',(19.5656042620897,-2.7384688239187,4.77296272555879));
#32938=CARTESIAN_POINT('Ctrl Pts',(19.057271160227,-2.57250304610006,4.26678755349543));
#32939=CARTESIAN_POINT('Ctrl Pts',(19.5173428295347,-2.5555887020504,4.26678755349543));
#32940=CARTESIAN_POINT('Ctrl Pts',(19.5575361035113,-2.54753565754633,4.72455016526169));
#32941=CARTESIAN_POINT('Ctrl Pts',(19.0269269806048,-2.24423104073317,4.26678755349543));
#32942=CARTESIAN_POINT('Ctrl Pts',(19.4037324746258,-2.19827110756716,4.26678755349543));
#32943=CARTESIAN_POINT('Ctrl Pts',(19.5066380987991,-2.17857853420919,4.63172588697633));
#32944=CARTESIAN_POINT('Ctrl Pts',(19.0011662279257,-2.0804291629179,4.26678755349543));
#32945=CARTESIAN_POINT('Ctrl Pts',(19.3411771890505,-2.0261294786292,4.26678755349543));
#32946=CARTESIAN_POINT('Ctrl Pts',(19.463348919041,-2.0002486625875,4.58724452357084));
#32947=CARTESIAN_POINT('Ctrl Pts',(18.9022612159307,-1.59259935669663,4.26678755349543));
#32948=CARTESIAN_POINT('Ctrl Pts',(19.1484414382609,-1.54317772475002,4.26678755349543));
#32949=CARTESIAN_POINT('Ctrl Pts',(19.2970255960277,-1.48543183133247,4.46381231351943));
#32950=CARTESIAN_POINT('Ctrl Pts',(18.808053085376,-1.27510872906614,4.26678755349543));
#32951=CARTESIAN_POINT('Ctrl Pts',(18.9991637252048,-1.22485530444607,4.26678755349543));
#32952=CARTESIAN_POINT('Ctrl Pts',(19.1384956426123,-1.17248948697599,4.39571969599962));
#32953=CARTESIAN_POINT('Ctrl Pts',(18.65499946014,-0.802082822629942,4.26678755349543));
#32954=CARTESIAN_POINT('Ctrl Pts',(18.7752857128794,-0.764203897240211,
4.26678755349543));
#32955=CARTESIAN_POINT('Ctrl Pts',(18.8808742045249,-0.726828291197418,
4.32500544029631));
#32956=CARTESIAN_POINT('Ctrl Pts',(18.6014509972622,-0.645096921999107,
4.26678755349543));
#32957=CARTESIAN_POINT('Ctrl Pts',(18.7002177320532,-0.613472528045095,
4.26678755349542));
#32958=CARTESIAN_POINT('Ctrl Pts',(18.7907282330956,-0.582301152819928,
4.30665226666321));
#32959=CARTESIAN_POINT('Ctrl Pts',(18.5277457016062,-0.407818315284438,
4.26678755349543));
#32960=CARTESIAN_POINT('Ctrl Pts',(18.598737077538,-0.387068822042169,4.26678755349543));
#32961=CARTESIAN_POINT('Ctrl Pts',(18.6666415536194,-0.366671419750548,
4.28784256921206));
#32962=CARTESIAN_POINT('Ctrl Pts',(18.5042426057228,-0.328435858715446,
4.26678755349543));
#32963=CARTESIAN_POINT('Ctrl Pts',(18.5666903059424,-0.311580987664372,
4.26678755349543));
#32964=CARTESIAN_POINT('Ctrl Pts',(18.6270715338758,-0.294994221998134,
4.28301860951388));
#32965=CARTESIAN_POINT('Ctrl Pts',(18.4373471175324,-0.0378434116184329,
4.26678755349543));
#32966=CARTESIAN_POINT('Ctrl Pts',(18.4761993712803,-0.0366262354591573,
4.26678755349543));
#32967=CARTESIAN_POINT('Ctrl Pts',(18.5144427309313,-0.0335231859295633,
4.27116249911528));
#32968=CARTESIAN_POINT('Ctrl Pts',(18.4253014419183,0.186125192633141,4.26678755349543));
#32969=CARTESIAN_POINT('Ctrl Pts',(18.4597225256734,0.17753430427652,4.26678755349789));
#32970=CARTESIAN_POINT('Ctrl Pts',(18.4941622956095,0.166269977993189,4.2728958886403));
#32971=CARTESIAN_POINT('Ctrl Pts',(18.5875304087241,0.411880125146817,4.26678755349542));
#32972=CARTESIAN_POINT('Ctrl Pts',(18.6805827233783,0.39133576211092,4.26678755348346));
#32973=CARTESIAN_POINT('Ctrl Pts',(18.7672955102272,0.370166055980356,4.28926970183153));
#32974=CARTESIAN_POINT('',(0.,0.,0.));
#32975=CARTESIAN_POINT('Origin',(0.,0.,0.));
#32976=CARTESIAN_POINT('',(-1.36919674566051E-15,-11.1803398874989,-10.));
#32977=CARTESIAN_POINT('',(-1.36919674566051E-15,-11.1803398874989,10.));
#32978=CARTESIAN_POINT('Origin',(0.,0.,0.));
#32979=CARTESIAN_POINT('',(11.1803398874989,0.,-10.));
#32980=CARTESIAN_POINT('Origin',(0.,0.,-10.));
#32981=CARTESIAN_POINT('',(11.1803398874989,0.,10.));
#32982=CARTESIAN_POINT('Origin',(11.1803398874989,0.,0.));
#32983=CARTESIAN_POINT('Origin',(0.,0.,10.));
#32984=CARTESIAN_POINT('Origin',(0.,0.,-10.));
#32985=CARTESIAN_POINT('',(-6.,-7.34788079488412E-16,-10.));
#32986=CARTESIAN_POINT('Origin',(0.,0.,-10.));
#32987=CARTESIAN_POINT('',(-6.,-7.34788079488412E-16,10.));
#32988=CARTESIAN_POINT('',(-6.,-7.34788079488412E-16,-10.));
#32989=CARTESIAN_POINT('Origin',(0.,0.,10.));
#32990=CARTESIAN_POINT('Origin',(0.,0.,0.));
#32991=CARTESIAN_POINT('Origin',(0.,0.,10.));
#32992=CARTESIAN_POINT('Origin',(11.1803398874989,0.,0.));
#32993=CARTESIAN_POINT('Origin',(0.,0.,-10.));
#32994=CARTESIAN_POINT('Origin',(140.,0.,0.));
#32995=CARTESIAN_POINT('',(140.,-4.89858719658941E-16,-4.));
#32996=CARTESIAN_POINT('',(140.,-4.89858719658941E-16,-4.));
#32997=CARTESIAN_POINT('Origin',(140.,0.,0.));
#32998=CARTESIAN_POINT('Origin',(-71.1905382258649,0.,0.));
#32999=CARTESIAN_POINT('',(149.5,-4.89858719658941E-16,-4.));
#33000=CARTESIAN_POINT('',(-71.1905382258649,-4.89858719658941E-16,-4.));
#33001=CARTESIAN_POINT('Origin',(149.5,0.,0.));
#33002=CARTESIAN_POINT('Origin',(150.,0.,0.));
#33003=CARTESIAN_POINT('',(150.,-4.28626379701574E-16,-3.5));
#33004=CARTESIAN_POINT('',(150.,-4.28626379701574E-16,-3.5));
#33005=CARTESIAN_POINT('Origin',(150.,0.,0.));
#33006=CARTESIAN_POINT('Origin',(150.,0.,0.));
#33007=CARTESIAN_POINT('Origin',(11.1803398874989,-15.,10.));
#33008=CARTESIAN_POINT('Origin',(11.1803398874989,-15.,-10.));
#33009=CARTESIAN_POINT('',(0.,0.,0.));
#33010=CARTESIAN_POINT('Origin',(2.,0.,0.));
#33011=CARTESIAN_POINT('',(2.,1.53080849893419E-15,-12.5));
#33012=CARTESIAN_POINT('',(2.,-1.53080849893419E-15,12.5));
#33013=CARTESIAN_POINT('Origin',(2.,0.,0.));
#33014=CARTESIAN_POINT('Origin',(2.,0.,0.));
#33015=CARTESIAN_POINT('',(0.,-1.28587913910472E-15,10.5));
#33016=CARTESIAN_POINT('Origin',(2.,-1.28587913910472E-15,10.5));
#33017=CARTESIAN_POINT('Origin',(0.,0.,0.));
#33018=CARTESIAN_POINT('Origin',(60.,0.,0.));
#33019=CARTESIAN_POINT('',(59.,-6.12323399573676E-16,-5.));
#33020=CARTESIAN_POINT('Origin',(59.,0.,0.));
#33021=CARTESIAN_POINT('',(60.,-5.20474889637625E-16,-4.25));
#33022=CARTESIAN_POINT('',(60.,-5.20474889637625E-16,-4.25));
#33023=CARTESIAN_POINT('Origin',(60.,0.,0.));
#33024=CARTESIAN_POINT('Origin',(0.,0.,0.));
#33025=CARTESIAN_POINT('',(50.0625,6.12323399573677E-16,5.));
#33026=CARTESIAN_POINT('',(50.0625,-6.12323399573677E-16,-5.));
#33027=CARTESIAN_POINT('Origin',(50.0625,0.,0.));
#33028=CARTESIAN_POINT('Origin',(50.0625,0.,0.));
#33029=CARTESIAN_POINT('',(0.,-6.12323399573677E-16,-5.));
#33030=CARTESIAN_POINT('Origin',(50.0625,0.,0.));
#33031=CARTESIAN_POINT('',(49.5,-5.20474889637625E-16,4.25));
#33032=CARTESIAN_POINT('',(50.0625,-6.12323399573677E-16,5.));
#33033=CARTESIAN_POINT('',(49.5,5.20474889637625E-16,-4.25));
#33034=CARTESIAN_POINT('Origin',(49.5,0.,0.));
#33035=CARTESIAN_POINT('Origin',(49.5,0.,0.));
#33036=CARTESIAN_POINT('Origin',(0.,0.,0.));
#33037=CARTESIAN_POINT('',(46.5,-5.20474889637625E-16,-4.25));
#33038=CARTESIAN_POINT('Origin',(46.5,0.,0.));
#33039=CARTESIAN_POINT('',(0.,-5.20474889637625E-16,-4.25));
#33040=CARTESIAN_POINT('Origin',(0.,0.,0.));
#33041=CARTESIAN_POINT('',(8.,-7.34788079488412E-16,-6.));
#33042=CARTESIAN_POINT('Origin',(8.,0.,0.));
#33043=CARTESIAN_POINT('',(46.5,-7.34788079488412E-16,-6.));
#33044=CARTESIAN_POINT('',(0.,-7.34788079488412E-16,-6.));
#33045=CARTESIAN_POINT('Origin',(46.5,0.,0.));
#33046=CARTESIAN_POINT('Origin',(0.,0.,0.));
#33047=CARTESIAN_POINT('',(8.,-1.53080849893419E-15,-12.5));
#33048=CARTESIAN_POINT('',(0.,-1.53080849893419E-15,-12.5));
#33049=CARTESIAN_POINT('Origin',(8.,0.,0.));
#33050=CARTESIAN_POINT('Origin',(0.,0.,0.));
#33051=CARTESIAN_POINT('Origin',(8.,12.5,0.));
#33052=CARTESIAN_POINT('Origin',(46.5,6.,0.));
#33053=CARTESIAN_POINT('Origin',(60.,4.25,0.));
#33054=CARTESIAN_POINT('',(0.,0.,0.));
#33055=CARTESIAN_POINT('Origin',(13.,12.5000000000006,-21.6506350946113));
#33056=CARTESIAN_POINT('',(13.,16.0623523599166,-16.8226287085547));
#33057=CARTESIAN_POINT('',(13.,6.5376476400841,-22.3217195425019));
#33058=CARTESIAN_POINT('Origin',(13.,12.5000000000006,-21.6506350946113));
#33059=CARTESIAN_POINT('',(15.,17.2498031465552,-15.2132932465359));
#33060=CARTESIAN_POINT('Origin',(13.,17.2498031465552,-15.2132932465359));
#33061=CARTESIAN_POINT('',(15.,4.55019685344533,-22.5454143584654));
#33062=CARTESIAN_POINT('Origin',(15.,12.5000000000006,-21.6506350946113));
#33063=CARTESIAN_POINT('Origin',(13.,4.55019685344533,-22.5454143584654));
#33064=CARTESIAN_POINT('Origin',(-8.28173040415688E-15,21.8,7.33212111192934));
#33065=CARTESIAN_POINT('',(2.,23.695652173913,7.96969686079276));
#33066=CARTESIAN_POINT('',(2.,22.6,5.49909083394701));
#33067=CARTESIAN_POINT('Origin',(2.,21.8,7.33212111192934));
#33068=CARTESIAN_POINT('',(13.,23.695652173913,7.96969686079277));
#33069=CARTESIAN_POINT('',(-2.90188045884916E-15,23.695652173913,7.96969686079276));
#33070=CARTESIAN_POINT('',(13.,22.6,5.49909083394701));
#33071=CARTESIAN_POINT('Origin',(13.,21.8,7.33212111192934));
#33072=CARTESIAN_POINT('',(-8.37970214808867E-15,22.6,5.49909083394701));
#33073=CARTESIAN_POINT('Origin',(13.,25.,0.));
#33074=CARTESIAN_POINT('',(13.,22.6,-5.49909083394701));
#33075=CARTESIAN_POINT('Origin',(13.,25.,0.));
#33076=CARTESIAN_POINT('',(15.,21.8,7.33212111192934));
#33077=CARTESIAN_POINT('Origin',(13.,21.8,7.33212111192934));
#33078=CARTESIAN_POINT('',(15.,21.8,-7.33212111192935));
#33079=CARTESIAN_POINT('Origin',(15.,25.,0.));
#33080=CARTESIAN_POINT('Origin',(13.,21.8,-7.33212111192934));
#33081=CARTESIAN_POINT('Origin',(2.,-12.4999999999994,-21.650635094612));
#33082=CARTESIAN_POINT('',(2.,-16.0623523599161,-16.822628708555));
#33083=CARTESIAN_POINT('',(2.,-6.53764764008211,-22.3217195425024));
#33084=CARTESIAN_POINT('Origin',(2.,-12.4999999999994,-21.650635094612));
#33085=CARTESIAN_POINT('',(3.84721509691184E-15,-17.2498031465548,-15.2132932465363));
#33086=CARTESIAN_POINT('Origin',(2.,-17.2498031465548,-15.2132932465363));
#33087=CARTESIAN_POINT('',(2.29196187718278E-15,-4.55019685344333,-22.5454143584658));
#33088=CARTESIAN_POINT('Origin',(3.46944695195361E-15,-12.4999999999994,
-21.650635094612));
#33089=CARTESIAN_POINT('Origin',(2.,-4.55019685344333,-22.5454143584658));
#33090=CARTESIAN_POINT('Origin',(-2.12661045170397E-15,-21.7999999999999,
7.33212111192955));
#33091=CARTESIAN_POINT('',(13.,-22.5999999999998,5.49909083394716));
#33092=CARTESIAN_POINT('',(13.,-23.695652173913,7.969696860793));
#33093=CARTESIAN_POINT('Origin',(13.,-21.7999999999999,7.33212111192956));
#33094=CARTESIAN_POINT('',(2.00000000000001,-23.695652173913,7.969696860793));
#33095=CARTESIAN_POINT('',(2.90188045884915E-15,-23.695652173913,7.96969686079299));
#33096=CARTESIAN_POINT('',(2.,-22.5999999999998,5.49909083394716));
#33097=CARTESIAN_POINT('Origin',(2.,-21.7999999999999,7.33212111192956));
#33098=CARTESIAN_POINT('',(-2.0286387077722E-15,-22.5999999999998,5.49909083394716));
#33099=CARTESIAN_POINT('Origin',(2.00000000000001,-25.,-1.4119006205266E-12));
#33100=CARTESIAN_POINT('',(2.,-22.5999999999992,-5.49909083394971));
#33101=CARTESIAN_POINT('Origin',(2.00000000000001,-25.,-1.4119006205266E-12));
#33102=CARTESIAN_POINT('',(4.40445349811803E-15,-21.7999999999999,7.33212111192956));
#33103=CARTESIAN_POINT('Origin',(2.,-21.7999999999999,7.33212111192956));
#33104=CARTESIAN_POINT('',(4.40445349811793E-15,-21.7999999999991,-7.33212111193202));
#33105=CARTESIAN_POINT('Origin',(4.77048955893622E-15,-25.,-1.4119006205266E-12));
#33106=CARTESIAN_POINT('Origin',(2.,-21.7999999999991,-7.33212111193202));
#33107=CARTESIAN_POINT('Origin',(-4.44301704968179E-15,-4.5501968534443,
22.5454143584656));
#33108=CARTESIAN_POINT('',(13.,-6.53764764008302,22.3217195425017));
#33109=CARTESIAN_POINT('',(13.,-4.94586614504815,24.5058851722452));
#33110=CARTESIAN_POINT('Origin',(13.,-4.5501968534443,22.5454143584656));
#33111=CARTESIAN_POINT('',(2.,-4.94586614504815,24.5058851722452));
#33112=CARTESIAN_POINT('',(6.05693914354447E-16,-4.94586614504815,24.5058851722452));
#33113=CARTESIAN_POINT('',(2.,-6.53764764008303,22.3217195425017));
#33114=CARTESIAN_POINT('Origin',(2.,-4.5501968534443,22.5454143584656));
#33115=CARTESIAN_POINT('',(-4.19962452524979E-15,-6.53764764008302,22.3217195425017));
#33116=CARTESIAN_POINT('Origin',(2.,-12.5000000000006,21.6506350946099));
#33117=CARTESIAN_POINT('',(2.,-16.062352359918,16.8226287085528));
#33118=CARTESIAN_POINT('Origin',(2.,-12.5000000000006,21.6506350946099));
#33119=CARTESIAN_POINT('',(2.2919618771829E-15,-4.5501968534443,22.5454143584656));
#33120=CARTESIAN_POINT('Origin',(2.,-4.5501968534443,22.5454143584656));
#33121=CARTESIAN_POINT('',(3.84721509691208E-15,-17.2498031465568,15.2132932465341));
#33122=CARTESIAN_POINT('Origin',(3.46944695195361E-15,-12.5000000000006,
21.6506350946099));
#33123=CARTESIAN_POINT('Origin',(2.,-17.2498031465568,15.2132932465341));
#33124=CARTESIAN_POINT('Origin',(13.,12.4999999999994,21.6506350946106));
#33125=CARTESIAN_POINT('',(13.,6.53764764008235,22.321719542502));
#33126=CARTESIAN_POINT('',(13.,16.0623523599166,16.8226287085542));
#33127=CARTESIAN_POINT('Origin',(13.,12.4999999999994,21.6506350946106));
#33128=CARTESIAN_POINT('',(15.,4.55019685344361,22.5454143584657));
#33129=CARTESIAN_POINT('Origin',(13.,4.55019685344361,22.5454143584657));
#33130=CARTESIAN_POINT('',(15.,17.2498031465555,15.2132932465356));
#33131=CARTESIAN_POINT('Origin',(15.,12.4999999999994,21.6506350946106));
#33132=CARTESIAN_POINT('Origin',(13.,17.2498031465555,15.2132932465355));
#33133=CARTESIAN_POINT('Origin',(-5.96532380617912E-15,4.55019685344361,
22.5454143584657));
#33134=CARTESIAN_POINT('',(2.,4.9458661450474,24.5058851722453));
#33135=CARTESIAN_POINT('',(2.,6.53764764008234,22.321719542502));
#33136=CARTESIAN_POINT('Origin',(2.,4.55019685344361,22.5454143584657));
#33137=CARTESIAN_POINT('',(13.,4.9458661450474,24.5058851722453));
#33138=CARTESIAN_POINT('',(-6.05693914354355E-16,4.9458661450474,24.5058851722453));
#33139=CARTESIAN_POINT('Origin',(13.,4.55019685344361,22.5454143584657));
#33140=CARTESIAN_POINT('',(-6.20871633061112E-15,6.53764764008235,22.321719542502));
#33141=CARTESIAN_POINT('Origin',(-3.46944695195361E-15,-12.5000000000006,
21.6506350946099));
#33142=CARTESIAN_POINT('',(13.,-16.062352359918,16.8226287085528));
#33143=CARTESIAN_POINT('',(-3.03318461045284E-15,-16.062352359918,16.8226287085528));
#33144=CARTESIAN_POINT('Origin',(13.,-12.5000000000006,21.6506350946099));
#33145=CARTESIAN_POINT('Origin',(-1.73472347597681E-15,-25.,-1.4119006205266E-12));
#33146=CARTESIAN_POINT('',(13.,-22.5999999999992,-5.49909083394971));
#33147=CARTESIAN_POINT('',(-2.02863870777227E-15,-22.5999999999992,-5.49909083394972));
#33148=CARTESIAN_POINT('Origin',(13.,-25.,-1.4119006205266E-12));
#33149=CARTESIAN_POINT('Origin',(-3.46944695195361E-15,-12.4999999999994,
-21.650635094612));
#33150=CARTESIAN_POINT('',(13.,-6.53764764008211,-22.3217195425024));
#33151=CARTESIAN_POINT('',(-4.19962452524975E-15,-6.53764764008211,-22.3217195425024));
#33152=CARTESIAN_POINT('',(13.,-16.0623523599161,-16.822628708555));
#33153=CARTESIAN_POINT('Origin',(13.,-12.4999999999994,-21.650635094612));
#33154=CARTESIAN_POINT('',(-3.03318461045291E-15,-16.0623523599161,-16.822628708555));
#33155=CARTESIAN_POINT('Origin',(0.,0.,0.));
#33156=CARTESIAN_POINT('',(30.,5.,-6.12323399573676E-16));
#33157=CARTESIAN_POINT('Origin',(30.,3.67394039744206E-15,0.));
#33158=CARTESIAN_POINT('',(18.,5.,-6.12323399573676E-16));
#33159=CARTESIAN_POINT('',(-6.12323399573676E-16,5.,-6.12323399573676E-16));
#33160=CARTESIAN_POINT('Origin',(18.,2.20436423846524E-15,0.));
#33161=CARTESIAN_POINT('Origin',(0.,0.,0.));
#33162=CARTESIAN_POINT('',(15.,12.5,-1.53080849893419E-15));
#33163=CARTESIAN_POINT('Origin',(15.,1.83697019872103E-15,0.));
#33164=CARTESIAN_POINT('',(30.,12.5,-1.53080849893419E-15));
#33165=CARTESIAN_POINT('',(-1.53080849893419E-15,12.5,-1.53080849893419E-15));
#33166=CARTESIAN_POINT('Origin',(30.,3.67394039744206E-15,0.));
#33167=CARTESIAN_POINT('Origin',(0.,0.,0.));
#33168=CARTESIAN_POINT('',(2.,18.7497860288644,-16.536188311452));
#33169=CARTESIAN_POINT('',(2.,23.695652173913,-7.96969686079276));
#33170=CARTESIAN_POINT('Origin',(2.,2.44929359829471E-16,0.));
#33171=CARTESIAN_POINT('',(13.,23.695652173913,-7.96969686079276));
#33172=CARTESIAN_POINT('',(-2.90188045884916E-15,23.695652173913,-7.96969686079276));
#33173=CARTESIAN_POINT('',(13.,18.7497860288644,-16.536188311452));
#33174=CARTESIAN_POINT('Origin',(13.,1.59204083889156E-15,0.));
#33175=CARTESIAN_POINT('',(-2.29618654449465E-15,18.7497860288644,-16.536188311452));
#33176=CARTESIAN_POINT('Origin',(0.,0.,0.));
#33177=CARTESIAN_POINT('',(2.,18.7497860288647,16.5361883114517));
#33178=CARTESIAN_POINT('Origin',(2.,2.44929359829471E-16,0.));
#33179=CARTESIAN_POINT('',(13.,18.7497860288647,16.5361883114517));
#33180=CARTESIAN_POINT('',(-2.29618654449469E-15,18.7497860288647,16.5361883114517));
#33181=CARTESIAN_POINT('Origin',(13.,1.59204083889156E-15,0.));
#33182=CARTESIAN_POINT('Origin',(0.,0.,0.));
#33183=CARTESIAN_POINT('Origin',(13.,1.59204083889156E-15,0.));
#33184=CARTESIAN_POINT('Origin',(2.,2.44929359829471E-16,0.));
#33185=CARTESIAN_POINT('Origin',(0.,0.,0.));
#33186=CARTESIAN_POINT('',(13.,-18.7497860288661,16.5361883114501));
#33187=CARTESIAN_POINT('Origin',(13.,1.59204083889156E-15,0.));
#33188=CARTESIAN_POINT('',(2.,-18.7497860288661,16.5361883114501));
#33189=CARTESIAN_POINT('',(2.29618654449486E-15,-18.7497860288661,16.5361883114501));
#33190=CARTESIAN_POINT('Origin',(2.,2.44929359829471E-16,0.));
#33191=CARTESIAN_POINT('Origin',(0.,0.,0.));
#33192=CARTESIAN_POINT('',(13.,-18.749786028864,-16.5361883114525));
#33193=CARTESIAN_POINT('',(13.,-23.6956521739121,-7.96969686079567));
#33194=CARTESIAN_POINT('Origin',(13.,1.59204083889156E-15,0.));
#33195=CARTESIAN_POINT('',(2.00000000000001,-23.6956521739121,-7.96969686079567));
#33196=CARTESIAN_POINT('',(2.90188045884904E-15,-23.6956521739121,-7.96969686079567));
#33197=CARTESIAN_POINT('',(2.,-18.7497860288639,-16.5361883114525));
#33198=CARTESIAN_POINT('Origin',(2.,2.44929359829471E-16,0.));
#33199=CARTESIAN_POINT('',(2.2961865444946E-15,-18.7497860288639,-16.5361883114525));
#33200=CARTESIAN_POINT('Origin',(2.,2.44929359829471E-16,0.));
#33201=CARTESIAN_POINT('',(-3.77768144958305E-16,17.2498031465555,15.2132932465355));
#33202=CARTESIAN_POINT('',(-9.35006546164422E-16,21.8,7.33212111192934));
#33203=CARTESIAN_POINT('Origin',(1.73472347597681E-15,2.40741243048404E-31,
0.));
#33204=CARTESIAN_POINT('Origin',(2.,17.2498031465555,15.2132932465355));
#33205=CARTESIAN_POINT('Origin',(2.,21.8,7.33212111192934));
#33206=CARTESIAN_POINT('Origin',(2.,2.44929359829471E-16,0.));
#33207=CARTESIAN_POINT('',(-9.35006546164422E-16,21.8,-7.33212111192934));
#33208=CARTESIAN_POINT('',(-3.77768144958272E-16,17.2498031465552,-15.2132932465359));
#33209=CARTESIAN_POINT('Origin',(1.73472347597681E-15,2.40741243048404E-31,
0.));
#33210=CARTESIAN_POINT('Origin',(2.,21.8,-7.33212111192934));
#33211=CARTESIAN_POINT('Origin',(2.,17.2498031465552,-15.2132932465359));
#33212=CARTESIAN_POINT('Origin',(2.,2.44929359829471E-16,0.));
#33213=CARTESIAN_POINT('',(1.1774850747708E-15,4.55019685344361,22.5454143584657));
#33214=CARTESIAN_POINT('Origin',(2.,4.55019685344361,22.5454143584657));
#33215=CARTESIAN_POINT('Origin',(1.73472347597681E-15,2.40741243048404E-31,
0.));
#33216=CARTESIAN_POINT('Origin',(2.,-4.5501968534443,22.5454143584656));
#33217=CARTESIAN_POINT('Origin',(2.,2.44929359829471E-16,0.));
#33218=CARTESIAN_POINT('Origin',(2.,-17.2498031465568,15.2132932465341));
#33219=CARTESIAN_POINT('Origin',(1.73472347597681E-15,2.40741243048404E-31,
0.));
#33220=CARTESIAN_POINT('Origin',(2.,-21.7999999999999,7.33212111192956));
#33221=CARTESIAN_POINT('Origin',(2.,2.44929359829471E-16,0.));
#33222=CARTESIAN_POINT('',(2.,-4.9458661450471,-24.5058851722454));
#33223=CARTESIAN_POINT('',(2.,4.94586614504927,-24.505885172245));
#33224=CARTESIAN_POINT('Origin',(2.,2.44929359829471E-16,0.));
#33225=CARTESIAN_POINT('Origin',(2.,-4.55019685344333,-22.5454143584658));
#33226=CARTESIAN_POINT('',(1.17748507477059E-15,4.55019685344533,-22.5454143584654));
#33227=CARTESIAN_POINT('Origin',(1.73472347597681E-15,2.40741243048404E-31,
0.));
#33228=CARTESIAN_POINT('Origin',(2.,4.55019685344533,-22.5454143584654));
#33229=CARTESIAN_POINT('Origin',(13.,1.59204083889156E-15,0.));
#33230=CARTESIAN_POINT('Origin',(13.,17.2498031465555,15.2132932465355));
#33231=CARTESIAN_POINT('Origin',(15.,1.83697019872103E-15,0.));
#33232=CARTESIAN_POINT('Origin',(13.,21.8,7.33212111192934));
#33233=CARTESIAN_POINT('Origin',(13.,1.59204083889156E-15,0.));
#33234=CARTESIAN_POINT('Origin',(13.,21.8,-7.33212111192934));
#33235=CARTESIAN_POINT('Origin',(15.,1.83697019872103E-15,0.));
#33236=CARTESIAN_POINT('Origin',(13.,17.2498031465552,-15.2132932465359));
#33237=CARTESIAN_POINT('Origin',(13.,1.59204083889156E-15,0.));
#33238=CARTESIAN_POINT('',(15.,-4.5501968534443,22.5454143584656));
#33239=CARTESIAN_POINT('Origin',(15.,1.83697019872103E-15,0.));
#33240=CARTESIAN_POINT('Origin',(13.,4.55019685344361,22.5454143584657));
#33241=CARTESIAN_POINT('Origin',(13.,-4.5501968534443,22.5454143584656));
#33242=CARTESIAN_POINT('Origin',(13.,1.59204083889156E-15,0.));
#33243=CARTESIAN_POINT('',(15.,-17.2498031465568,15.2132932465341));
#33244=CARTESIAN_POINT('',(15.,-21.7999999999999,7.33212111192955));
#33245=CARTESIAN_POINT('Origin',(15.,1.83697019872103E-15,0.));
#33246=CARTESIAN_POINT('Origin',(13.,-17.2498031465568,15.2132932465341));
#33247=CARTESIAN_POINT('Origin',(13.,-21.7999999999999,7.33212111192956));
#33248=CARTESIAN_POINT('Origin',(13.,1.59204083889156E-15,0.));
#33249=CARTESIAN_POINT('',(15.,-4.55019685344333,-22.5454143584658));
#33250=CARTESIAN_POINT('Origin',(15.,1.83697019872103E-15,0.));
#33251=CARTESIAN_POINT('',(13.,-4.94586614504711,-24.5058851722454));
#33252=CARTESIAN_POINT('Origin',(13.,-4.55019685344333,-22.5454143584658));
#33253=CARTESIAN_POINT('',(13.,4.94586614504927,-24.505885172245));
#33254=CARTESIAN_POINT('Origin',(13.,1.59204083889156E-15,0.));
#33255=CARTESIAN_POINT('Origin',(13.,4.55019685344533,-22.5454143584654));
#33256=CARTESIAN_POINT('Origin',(1.53080849893419E-15,1.87469972832732E-31,
0.));
#33257=CARTESIAN_POINT('Origin',(0.,12.4999999999994,21.6506350946106));
#33258=CARTESIAN_POINT('Origin',(-1.30104260698261E-15,25.,0.));
#33259=CARTESIAN_POINT('Origin',(0.,12.5000000000006,-21.6506350946113));
#33260=CARTESIAN_POINT('Origin',(1.73472347597681E-15,2.40741243048404E-31,
0.));
#33261=CARTESIAN_POINT('Origin',(0.,0.,0.));
#33262=CARTESIAN_POINT('',(6.05693914354321E-16,-4.94586614504712,-24.5058851722454));
#33263=CARTESIAN_POINT('',(-6.05693914354585E-16,4.94586614504927,-24.505885172245));
#33264=CARTESIAN_POINT('Origin',(15.,25.,0.));
#33265=CARTESIAN_POINT('Origin',(15.,-12.5000000000006,21.6506350946099));
#33266=CARTESIAN_POINT('',(15.,-21.7999999999991,-7.33212111193202));
#33267=CARTESIAN_POINT('Origin',(15.,-25.,-1.4119006205266E-12));
#33268=CARTESIAN_POINT('',(15.,-17.2498031465548,-15.2132932465363));
#33269=CARTESIAN_POINT('Origin',(15.,1.83697019872103E-15,0.));
#33270=CARTESIAN_POINT('Origin',(15.,-12.4999999999994,-21.650635094612));
#33271=CARTESIAN_POINT('Origin',(30.,12.5,0.));
#33272=CARTESIAN_POINT('Origin',(18.,5.,0.));
#33273=CARTESIAN_POINT('Origin',(2.,2.44929359829471E-16,0.));
#33274=CARTESIAN_POINT('Origin',(2.,-21.7999999999991,-7.33212111193202));
#33275=CARTESIAN_POINT('Origin',(2.,-17.2498031465548,-15.2132932465363));
#33276=CARTESIAN_POINT('Origin',(13.,1.59204083889156E-15,0.));
#33277=CARTESIAN_POINT('Origin',(13.,-21.7999999999991,-7.33212111193202));
#33278=CARTESIAN_POINT('Origin',(13.,-17.2498031465548,-15.2132932465363));
#33279=CARTESIAN_POINT('Origin',(-6.93889390390723E-15,12.5000000000006,
-21.6506350946113));
#33280=CARTESIAN_POINT('',(2.,6.5376476400841,-22.3217195425019));
#33281=CARTESIAN_POINT('',(-6.20871633061119E-15,6.5376476400841,-22.3217195425019));
#33282=CARTESIAN_POINT('',(2.,16.0623523599166,-16.8226287085547));
#33283=CARTESIAN_POINT('Origin',(2.,12.5000000000006,-21.6506350946113));
#33284=CARTESIAN_POINT('',(-7.37515624540784E-15,16.0623523599166,-16.8226287085547));
#33285=CARTESIAN_POINT('Origin',(-6.93889390390723E-15,12.4999999999994,
21.6506350946106));
#33286=CARTESIAN_POINT('',(2.,16.0623523599166,16.8226287085542));
#33287=CARTESIAN_POINT('',(-7.37515624540799E-15,16.0623523599166,16.8226287085542));
#33288=CARTESIAN_POINT('Origin',(2.,12.4999999999994,21.6506350946106));
#33289=CARTESIAN_POINT('Origin',(-8.67361737988404E-15,25.,0.));
#33290=CARTESIAN_POINT('',(2.,22.6,-5.49909083394701));
#33291=CARTESIAN_POINT('',(-8.37970214808867E-15,22.6,-5.49909083394701));
#33292=CARTESIAN_POINT('Origin',(2.,25.,0.));
#33293=CARTESIAN_POINT('Origin',(2.,4.55019685344361,22.5454143584657));
#33294=CARTESIAN_POINT('Origin',(2.,4.55019685344361,22.5454143584657));
#33295=CARTESIAN_POINT('Origin',(13.,4.55019685344361,22.5454143584657));
#33296=CARTESIAN_POINT('Origin',(2.,12.4999999999994,21.6506350946106));
#33297=CARTESIAN_POINT('Origin',(2.,17.2498031465555,15.2132932465355));
#33298=CARTESIAN_POINT('Origin',(2.,17.2498031465555,15.2132932465355));
#33299=CARTESIAN_POINT('Origin',(2.,17.2498031465555,15.2132932465355));
#33300=CARTESIAN_POINT('Origin',(13.,17.2498031465555,15.2132932465355));
#33301=CARTESIAN_POINT('Origin',(13.,17.2498031465555,15.2132932465355));
#33302=CARTESIAN_POINT('Origin',(-7.52057702590823E-15,17.2498031465555,
15.2132932465355));
#33303=CARTESIAN_POINT('Origin',(-2.88776382995261E-15,-17.2498031465568,
15.2132932465341));
#33304=CARTESIAN_POINT('Origin',(2.,-17.2498031465568,15.2132932465341));
#33305=CARTESIAN_POINT('Origin',(13.,-17.2498031465568,15.2132932465341));
#33306=CARTESIAN_POINT('Origin',(2.,-17.2498031465568,15.2132932465341));
#33307=CARTESIAN_POINT('Origin',(13.,-17.2498031465568,15.2132932465341));
#33308=CARTESIAN_POINT('Origin',(13.,-17.2498031465568,15.2132932465341));
#33309=CARTESIAN_POINT('Origin',(13.,-12.5000000000006,21.6506350946099));
#33310=CARTESIAN_POINT('Origin',(13.,-4.5501968534443,22.5454143584656));
#33311=CARTESIAN_POINT('Origin',(2.,-4.5501968534443,22.5454143584656));
#33312=CARTESIAN_POINT('Origin',(13.,-4.5501968534443,22.5454143584656));
#33313=CARTESIAN_POINT('Origin',(-2.12661045170407E-15,-21.7999999999991,
-7.33212111193201));
#33314=CARTESIAN_POINT('Origin',(2.,-21.7999999999991,-7.33212111193201));
#33315=CARTESIAN_POINT('Origin',(13.,-21.7999999999991,-7.33212111193202));
#33316=CARTESIAN_POINT('Origin',(2.,-21.7999999999991,-7.33212111193202));
#33317=CARTESIAN_POINT('Origin',(13.,-21.7999999999991,-7.33212111193202));
#33318=CARTESIAN_POINT('Origin',(13.,-21.7999999999991,-7.33212111193202));
#33319=CARTESIAN_POINT('Origin',(13.,-25.,-1.4119006205266E-12));
#33320=CARTESIAN_POINT('Origin',(13.,-21.7999999999999,7.33212111192956));
#33321=CARTESIAN_POINT('Origin',(2.,-21.7999999999999,7.33212111192956));
#33322=CARTESIAN_POINT('Origin',(13.,-21.7999999999999,7.33212111192956));
#33323=CARTESIAN_POINT('Origin',(13.,-12.4999999999994,-21.650635094612));
#33324=CARTESIAN_POINT('Origin',(13.,-4.55019685344333,-22.5454143584658));
#33325=CARTESIAN_POINT('Origin',(13.,-17.2498031465548,-15.2132932465363));
#33326=CARTESIAN_POINT('Origin',(13.,-4.55019685344333,-22.5454143584658));
#33327=CARTESIAN_POINT('Origin',(13.,-4.55019685344333,-22.5454143584658));
#33328=CARTESIAN_POINT('Origin',(13.,-17.2498031465548,-15.2132932465363));
#33329=CARTESIAN_POINT('Origin',(13.,-17.2498031465548,-15.2132932465363));
#33330=CARTESIAN_POINT('Origin',(-4.44301704968176E-15,-4.55019685344334,
-22.5454143584658));
#33331=CARTESIAN_POINT('Origin',(2.,-4.55019685344334,-22.5454143584658));
#33332=CARTESIAN_POINT('Origin',(-2.8877638299527E-15,-17.2498031465548,
-15.2132932465363));
#33333=CARTESIAN_POINT('Origin',(2.,-17.2498031465548,-15.2132932465363));
#33334=CARTESIAN_POINT('Origin',(2.,-4.55019685344333,-22.5454143584658));
#33335=CARTESIAN_POINT('Origin',(2.,-17.2498031465548,-15.2132932465363));
#33336=CARTESIAN_POINT('Origin',(13.,21.8,7.33212111192934));
#33337=CARTESIAN_POINT('Origin',(13.,21.8,-7.33212111192934));
#33338=CARTESIAN_POINT('Origin',(13.,21.8,-7.33212111192934));
#33339=CARTESIAN_POINT('Origin',(-8.28173040415688E-15,21.8,-7.33212111192934));
#33340=CARTESIAN_POINT('Origin',(2.,21.8,-7.33212111192934));
#33341=CARTESIAN_POINT('Origin',(2.,21.8,7.33212111192934));
#33342=CARTESIAN_POINT('Origin',(2.,21.8,7.33212111192934));
#33343=CARTESIAN_POINT('Origin',(2.,21.8,-7.33212111192934));
#33344=CARTESIAN_POINT('Origin',(2.,21.8,-7.33212111192934));
#33345=CARTESIAN_POINT('Origin',(2.,25.,0.));
#33346=CARTESIAN_POINT('Origin',(13.,17.2498031465552,-15.2132932465359));
#33347=CARTESIAN_POINT('Origin',(13.,17.2498031465552,-15.2132932465359));
#33348=CARTESIAN_POINT('Origin',(13.,4.55019685344533,-22.5454143584654));
#33349=CARTESIAN_POINT('Origin',(13.,4.55019685344533,-22.5454143584654));
#33350=CARTESIAN_POINT('Origin',(-7.52057702590804E-15,17.2498031465552,
-15.2132932465359));
#33351=CARTESIAN_POINT('Origin',(2.,17.2498031465552,-15.2132932465359));
#33352=CARTESIAN_POINT('Origin',(-5.96532380617918E-15,4.55019685344533,
-22.5454143584654));
#33353=CARTESIAN_POINT('Origin',(2.,4.55019685344533,-22.5454143584654));
#33354=CARTESIAN_POINT('Origin',(2.,17.2498031465552,-15.2132932465359));
#33355=CARTESIAN_POINT('Origin',(2.,17.2498031465552,-15.2132932465359));
#33356=CARTESIAN_POINT('Origin',(2.,4.55019685344533,-22.5454143584654));
#33357=CARTESIAN_POINT('Origin',(2.,4.55019685344533,-22.5454143584654));
#33358=CARTESIAN_POINT('Origin',(2.,12.5000000000006,-21.6506350946113));
#33359=CARTESIAN_POINT('',(0.,0.,0.));
#33360=CARTESIAN_POINT('Origin',(16.1460502915689,43.6543320991532,35.0294657090004));
#33361=CARTESIAN_POINT('',(16.1460502915689,43.6543320991532,33.0294657090004));
#33362=CARTESIAN_POINT('Origin',(16.1460502915689,43.6543320991532,35.0294657090004));
#33363=CARTESIAN_POINT('',(16.1460502915689,43.9543320991532,32.7294657090004));
#33364=CARTESIAN_POINT('',(16.1460502915689,43.6543320991532,33.0294657090004));
#33365=CARTESIAN_POINT('Origin',(16.1460502915689,43.9543320991532,35.0294657090004));
#33366=CARTESIAN_POINT('Origin',(43.4397894030341,37.9543320991532,35.0294657090004));
#33367=CARTESIAN_POINT('',(44.9397894030341,37.9543320991532,34.7294657090003));
#33368=CARTESIAN_POINT('',(41.9397894030341,37.9543320991532,34.7294657090003));
#33369=CARTESIAN_POINT('Origin',(43.4397894030341,37.9543320991532,34.7294657090003));
#33370=CARTESIAN_POINT('Origin',(43.4397894030341,37.9543320991532,34.7294657090003));
#33371=CARTESIAN_POINT('',(41.6397894030341,37.9543320991532,35.0294657090004));
#33372=CARTESIAN_POINT('',(41.6397894030341,37.9543320991532,35.0294657090004));
#33373=CARTESIAN_POINT('Origin',(43.4397894030341,37.9543320991532,35.0294657090004));
#33374=CARTESIAN_POINT('Origin',(54.9397894030341,37.9543320991532,35.0294657090004));
#33375=CARTESIAN_POINT('',(56.9397894030341,37.9543320991532,34.7294657090004));
#33376=CARTESIAN_POINT('',(52.9397894030341,37.9543320991532,34.7294657090004));
#33377=CARTESIAN_POINT('Origin',(54.9397894030341,37.9543320991532,34.7294657090004));
#33378=CARTESIAN_POINT('Origin',(54.9397894030341,37.9543320991532,34.7294657090004));
#33379=CARTESIAN_POINT('',(52.6397894030341,37.9543320991532,35.0294657090004));
#33380=CARTESIAN_POINT('',(52.6397894030341,37.9543320991532,35.0294657090004));
#33381=CARTESIAN_POINT('Origin',(54.9397894030341,37.9543320991532,35.0294657090004));
#33382=CARTESIAN_POINT('Origin',(35.9397894030341,41.6543320991532,38.5294657090004));
#33383=CARTESIAN_POINT('',(35.9397894030341,41.6543320991532,37.3294657090004));
#33384=CARTESIAN_POINT('Origin',(35.9397894030341,41.6543320991532,38.5294657090004));
#33385=CARTESIAN_POINT('',(35.9397894030341,41.9543320991532,37.0294657090003));
#33386=CARTESIAN_POINT('',(35.9397894030341,41.6543320991532,37.3294657090004));
#33387=CARTESIAN_POINT('Origin',(35.9397894030341,41.9543320991532,38.5294657090004));
#33388=CARTESIAN_POINT('Origin',(20.9397894030341,36.0543320991532,41.0294657090004));
#33389=CARTESIAN_POINT('',(17.9535710587063,37.2043320991532,40.7294657090004));
#33390=CARTESIAN_POINT('',(19.1460502915689,38.7043320991532,40.7294657090004));
#33391=CARTESIAN_POINT('Origin',(20.9397894030341,36.0543320991532,40.7294657090004));
#33392=CARTESIAN_POINT('',(17.634112467821,37.2043320991532,41.0294657090004));
#33393=CARTESIAN_POINT('Ctrl Pts',(17.6341124678211,37.2043320991532,41.0294657090003));
#33394=CARTESIAN_POINT('Ctrl Pts',(17.8009938212686,37.2043320991532,40.8718497544264));
#33395=CARTESIAN_POINT('Ctrl Pts',(17.9535710587063,37.2043320991532,40.7294657090004));
#33396=CARTESIAN_POINT('',(18.6534167299994,38.7043320991532,41.0294657090004));
#33397=CARTESIAN_POINT('Origin',(20.9397894030341,36.0543320991532,41.0294657090004));
#33398=CARTESIAN_POINT('Ctrl Pts',(19.1460502915689,38.7043320991532,40.7294657090004));
#33399=CARTESIAN_POINT('Ctrl Pts',(18.9107626203695,38.7043320991532,40.8613546772117));
#33400=CARTESIAN_POINT('Ctrl Pts',(18.6534167299948,38.7043320991532,41.0294657090034));
#33401=CARTESIAN_POINT('Origin',(35.9397894030341,33.9543320991532,38.5294657090004));
#33402=CARTESIAN_POINT('',(35.9397894030341,34.2543320991532,37.3294657090004));
#33403=CARTESIAN_POINT('',(35.9397894030341,34.2543320991532,39.7294657090004));
#33404=CARTESIAN_POINT('Origin',(35.9397894030341,34.2543320991532,38.5294657090004));
#33405=CARTESIAN_POINT('Origin',(35.9397894030341,34.2543320991532,38.5294657090004));
#33406=CARTESIAN_POINT('',(35.9397894030341,33.9543320991532,40.0294657090004));
#33407=CARTESIAN_POINT('',(35.9397894030341,33.9543320991532,40.0294657090004));
#33408=CARTESIAN_POINT('Origin',(35.9397894030341,33.9543320991532,38.5294657090004));
#33409=CARTESIAN_POINT('Origin',(16.1460502915689,31.9543320991532,35.0294657090004));
#33410=CARTESIAN_POINT('',(16.1460502915689,32.2543320991532,33.0294657090004));
#33411=CARTESIAN_POINT('',(16.1460502915689,32.2543320991532,37.0294657090004));
#33412=CARTESIAN_POINT('Origin',(16.1460502915689,32.2543320991532,35.0294657090004));
#33413=CARTESIAN_POINT('Origin',(16.1460502915689,32.2543320991532,35.0294657090004));
#33414=CARTESIAN_POINT('',(16.1460502915689,31.9543320991532,37.3294657090004));
#33415=CARTESIAN_POINT('',(16.1460502915689,31.9543320991532,37.3294657090004));
#33416=CARTESIAN_POINT('Origin',(16.1460502915689,31.9543320991532,35.0294657090004));
#33417=CARTESIAN_POINT('Origin',(54.9397894030341,37.9543320991532,29.3294657090003));
#33418=CARTESIAN_POINT('',(56.9397894030341,37.9543320991532,29.3294657090003));
#33419=CARTESIAN_POINT('Origin',(54.9397894030341,37.9543320991532,29.3294657090003));
#33420=CARTESIAN_POINT('',(57.2397894030341,37.9543320991532,29.0294657090004));
#33421=CARTESIAN_POINT('',(56.9397894030341,37.9543320991532,29.3294657090003));
#33422=CARTESIAN_POINT('Origin',(54.9397894030341,37.9543320991532,29.0294657090004));
#33423=CARTESIAN_POINT('Origin',(43.4397894030341,37.9543320991532,29.3294657090004));
#33424=CARTESIAN_POINT('',(44.9397894030341,37.9543320991532,29.3294657090004));
#33425=CARTESIAN_POINT('Origin',(43.4397894030341,37.9543320991532,29.3294657090004));
#33426=CARTESIAN_POINT('',(45.2397894030341,37.9543320991532,29.0294657090004));
#33427=CARTESIAN_POINT('',(44.9397894030341,37.9543320991532,29.3294657090004));
#33428=CARTESIAN_POINT('Origin',(43.4397894030341,37.9543320991532,29.0294657090004));
#33429=CARTESIAN_POINT('Origin',(20.9397894030341,36.0543320991532,29.3294657090004));
#33430=CARTESIAN_POINT('',(19.1460502915689,38.7043320991532,29.3294657090004));
#33431=CARTESIAN_POINT('',(17.9535710587063,37.2043320991532,29.3294657090004));
#33432=CARTESIAN_POINT('Origin',(20.9397894030341,36.0543320991532,29.3294657090004));
#33433=CARTESIAN_POINT('',(18.6534167299994,38.7043320991532,29.0294657090004));
#33434=CARTESIAN_POINT('Ctrl Pts',(18.6534167299948,38.7043320991532,29.0294657089973));
#33435=CARTESIAN_POINT('Ctrl Pts',(18.9107626203694,38.7043320991532,29.1975767407891));
#33436=CARTESIAN_POINT('Ctrl Pts',(19.1460502915689,38.7043320991532,29.3294657090004));
#33437=CARTESIAN_POINT('',(17.634112467821,37.2043320991532,29.0294657090004));
#33438=CARTESIAN_POINT('Origin',(20.9397894030341,36.0543320991532,29.0294657090004));
#33439=CARTESIAN_POINT('Ctrl Pts',(17.9535710587063,37.2043320991532,29.3294657090003));
#33440=CARTESIAN_POINT('Ctrl Pts',(17.8009938212686,37.2043320991532,29.1870816635743));
#33441=CARTESIAN_POINT('Ctrl Pts',(17.6341124678211,37.2043320991532,29.0294657090004));
#33442=CARTESIAN_POINT('Origin',(16.1460502915689,31.9543320991532,35.0294657090004));
#33443=CARTESIAN_POINT('',(16.1460502915689,37.2043320991532,33.0294657090004));
#33444=CARTESIAN_POINT('',(16.1460502915689,31.9543320991532,33.0294657090004));
#33445=CARTESIAN_POINT('',(17.9535710587063,37.2043320991532,35.8855432033705));
#33446=CARTESIAN_POINT('Origin',(16.1460502915689,37.2043320991532,35.0294657090004));
#33447=CARTESIAN_POINT('',(17.9535710587063,37.2043320991532,34.1733882146302));
#33448=CARTESIAN_POINT('Ctrl Pts',(17.9535710587063,37.2043320991532,35.8855432033705));
#33449=CARTESIAN_POINT('Ctrl Pts',(17.9192709480126,37.1152646037045,35.9579644068266));
#33450=CARTESIAN_POINT('Ctrl Pts',(17.8836292597541,37.0084958974654,36.0212420504143));
#33451=CARTESIAN_POINT('Ctrl Pts',(17.7876418033145,36.6624002842562,36.1795322193216));
#33452=CARTESIAN_POINT('Ctrl Pts',(17.7397894030341,36.3346151799028,36.2377685040754));
#33453=CARTESIAN_POINT('Ctrl Pts',(17.7397894030341,35.7740490184036,36.2377685040754));
#33454=CARTESIAN_POINT('Ctrl Pts',(17.7876418033145,35.4462639140502,36.1795322193216));
#33455=CARTESIAN_POINT('Ctrl Pts',(17.8925030363182,35.0681727125076,36.0066085592971));
#33456=CARTESIAN_POINT('Ctrl Pts',(17.9435339040124,34.9253475867885,35.9130653773292));
#33457=CARTESIAN_POINT('Ctrl Pts',(18.0267768582634,34.7255600011841,35.7177393279079));
#33458=CARTESIAN_POINT('Ctrl Pts',(18.069284710185,34.6385464913584,35.5957227639568));
#33459=CARTESIAN_POINT('Ctrl Pts',(18.1292923320046,34.522878497267,35.3231165996605));
#33460=CARTESIAN_POINT('Ctrl Pts',(18.1460502915689,34.4938764679129,35.1725117883411));
#33461=CARTESIAN_POINT('Ctrl Pts',(18.1460502915689,34.4938764679129,35.0294657090004));
#33462=CARTESIAN_POINT('Ctrl Pts',(18.1460502915689,34.4938764679129,34.8864196296597));
#33463=CARTESIAN_POINT('Ctrl Pts',(18.1292923320046,34.522878497267,34.7358148183402));
#33464=CARTESIAN_POINT('Ctrl Pts',(18.069284710185,34.6385464913584,34.463208654044));
#33465=CARTESIAN_POINT('Ctrl Pts',(18.0267768582634,34.7255600011841,34.3411920900928));
#33466=CARTESIAN_POINT('Ctrl Pts',(17.9435339040124,34.9253475867885,34.1458660406716));
#33467=CARTESIAN_POINT('Ctrl Pts',(17.8925030363182,35.0681727125076,34.0523228587036));
#33468=CARTESIAN_POINT('Ctrl Pts',(17.7876418033145,35.4462639140502,33.8793991986791));
#33469=CARTESIAN_POINT('Ctrl Pts',(17.7397894030341,35.7740490184036,33.8211629139253));
#33470=CARTESIAN_POINT('Ctrl Pts',(17.7397894030341,36.3346151799028,33.8211629139253));
#33471=CARTESIAN_POINT('Ctrl Pts',(17.7876418033145,36.6624002842562,33.8793991986791));
#33472=CARTESIAN_POINT('Ctrl Pts',(17.8836292597541,37.0084958974654,34.0376893675864));
#33473=CARTESIAN_POINT('Ctrl Pts',(17.9192709480126,37.1152646037045,34.1009670111741));
#33474=CARTESIAN_POINT('Ctrl Pts',(17.9535710587063,37.2043320991532,34.1733882146302));
#33475=CARTESIAN_POINT('Origin',(16.1460502915689,37.2043320991532,35.0294657090004));
#33476=CARTESIAN_POINT('Origin',(16.1460502915689,31.9543320991532,35.0294657090004));
#33477=CARTESIAN_POINT('',(16.1460502915689,38.7043320991532,33.0294657090004));
#33478=CARTESIAN_POINT('Origin',(16.1460502915689,38.7043320991532,35.0294657090004));
#33479=CARTESIAN_POINT('',(16.1460502915689,31.9543320991532,33.0294657090004));
#33480=CARTESIAN_POINT('Origin',(35.9397894030341,31.9543320991532,38.5294657090004));
#33481=CARTESIAN_POINT('',(35.9397894030341,31.9543320991532,37.3294657090004));
#33482=CARTESIAN_POINT('Origin',(20.9397894030341,36.0543320991532,41.0294657090004));
#33483=CARTESIAN_POINT('',(19.1460502915689,38.7043320991532,41.0294657090004));
#33484=CARTESIAN_POINT('',(17.9535710587063,37.2043320991532,41.0294657090004));
#33485=CARTESIAN_POINT('',(17.9535710587063,37.2043320991532,41.0294657090004));
#33486=CARTESIAN_POINT('Origin',(54.9397894030341,37.9543320991532,41.0294657090004));
#33487=CARTESIAN_POINT('',(56.9397894030341,37.9543320991532,41.0294657090004));
#33488=CARTESIAN_POINT('Origin',(43.4397894030341,37.9543320991532,41.0294657090004));
#33489=CARTESIAN_POINT('',(44.9397894030341,37.9543320991532,41.0294657090004));
#33490=CARTESIAN_POINT('Origin',(0.939789403034137,43.9543320991532,41.0294657090004));
#33491=CARTESIAN_POINT('',(0.939789403034137,43.6543320991532,41.0294657090004));
#33492=CARTESIAN_POINT('',(0.939789403034137,39.9843320991532,41.0294657090004));
#33493=CARTESIAN_POINT('',(0.939789403034137,43.9543320991532,41.0294657090004));
#33494=CARTESIAN_POINT('',(0.939789403034137,43.6543320991532,29.0294657090004));
#33495=CARTESIAN_POINT('',(0.939789403034137,43.6543320991532,41.0294657090004));
#33496=CARTESIAN_POINT('',(0.939789403034137,39.9843320991532,29.0294657090004));
#33497=CARTESIAN_POINT('',(0.939789403034137,43.9543320991532,29.0294657090004));
#33498=CARTESIAN_POINT('',(0.939789403034137,39.9843320991532,41.0294657090004));
#33499=CARTESIAN_POINT('Origin',(60.9397894030341,43.9543320991532,35.0294657090004));
#33500=CARTESIAN_POINT('',(60.9397894030341,43.6543320991532,29.3294657090004));
#33501=CARTESIAN_POINT('',(60.9397894030341,43.6543320991532,34.7294657090004));
#33502=CARTESIAN_POINT('',(60.9397894030341,43.6543320991532,35.0294657090004));
#33503=CARTESIAN_POINT('',(60.9397894030341,32.2543320991532,34.7294657090004));
#33504=CARTESIAN_POINT('',(60.9397894030341,43.9543320991532,34.7294657090004));
#33505=CARTESIAN_POINT('',(60.9397894030341,32.2543320991532,29.3294657090004));
#33506=CARTESIAN_POINT('',(60.9397894030341,32.2543320991532,29.0294657090004));
#33507=CARTESIAN_POINT('',(60.9397894030341,43.9543320991532,29.3294657090004));
#33508=CARTESIAN_POINT('Origin',(0.939789403034137,43.9543320991532,29.0294657090004));
#33509=CARTESIAN_POINT('',(13.1738772623021,38.7043320991532,29.0294657090004));
#33510=CARTESIAN_POINT('',(19.1460502915689,38.7043320991532,29.0294657090004));
#33511=CARTESIAN_POINT('',(4.70570154376622,38.7043320991532,29.0294657090004));
#33512=CARTESIAN_POINT('Origin',(8.93978940303414,37.9543320991532,29.0294657090004));
#33513=CARTESIAN_POINT('',(2.61978940303414,38.7043320991532,29.0294657090004));
#33514=CARTESIAN_POINT('',(5.01073099165871,38.7043320991532,29.0294657090004));
#33515=CARTESIAN_POINT('',(2.61978940303414,40.9543320991532,29.0294657090004));
#33516=CARTESIAN_POINT('',(2.61978940303414,40.9543320991532,29.0294657090004));
#33517=CARTESIAN_POINT('',(0.939789403034137,39.9843320991532,29.0294657090004));
#33518=CARTESIAN_POINT('',(60.6397894030341,43.6543320991532,29.0294657090004));
#33519=CARTESIAN_POINT('',(0.939789403034137,43.6543320991532,29.0294657090004));
#33520=CARTESIAN_POINT('',(60.6397894030341,32.2543320991532,29.0294657090004));
#33521=CARTESIAN_POINT('',(60.6397894030341,43.9543320991532,29.0294657090004));
#33522=CARTESIAN_POINT('',(0.939789403034137,32.2543320991532,29.0294657090004));
#33523=CARTESIAN_POINT('',(0.939789403034137,32.2543320991532,29.0294657090004));
#33524=CARTESIAN_POINT('',(0.939789403034137,35.9243320991532,29.0294657090004));
#33525=CARTESIAN_POINT('',(0.939789403034137,43.9543320991532,29.0294657090004));
#33526=CARTESIAN_POINT('',(2.61978940303414,34.9543320991532,29.0294657090004));
#33527=CARTESIAN_POINT('',(2.61978940303414,34.9543320991532,29.0294657090004));
#33528=CARTESIAN_POINT('',(2.61978940303414,37.2043320991532,29.0294657090004));
#33529=CARTESIAN_POINT('',(2.61978940303414,37.2043320991532,29.0294657090004));
#33530=CARTESIAN_POINT('',(4.70570154376622,37.2043320991532,29.0294657090004));
#33531=CARTESIAN_POINT('',(5.01073099165871,37.2043320991532,29.0294657090004));
#33532=CARTESIAN_POINT('',(13.1738772623021,37.2043320991532,29.0294657090004));
#33533=CARTESIAN_POINT('Origin',(8.93978940303414,37.9543320991532,29.0294657090004));
#33534=CARTESIAN_POINT('',(17.9535710587063,37.2043320991532,29.0294657090004));
#33535=CARTESIAN_POINT('Origin',(0.939789403034137,43.9543320991532,41.0294657090004));
#33536=CARTESIAN_POINT('',(0.939789403034137,32.2543320991532,41.0294657090004));
#33537=CARTESIAN_POINT('',(0.939789403034137,32.2543320991532,41.0294657090004));
#33538=CARTESIAN_POINT('',(0.939789403034137,35.9243320991532,41.0294657090004));
#33539=CARTESIAN_POINT('',(0.939789403034137,43.9543320991532,41.0294657090004));
#33540=CARTESIAN_POINT('',(0.939789403034137,35.9243320991532,41.0294657090004));
#33541=CARTESIAN_POINT('Origin',(0.939789403034137,43.9543320991532,41.0294657090004));
#33542=CARTESIAN_POINT('',(13.173877262302,38.7043320991532,41.0294657090004));
#33543=CARTESIAN_POINT('',(19.1460502915689,38.7043320991532,41.0294657090004));
#33544=CARTESIAN_POINT('',(13.173877262302,37.2043320991532,41.0294657090004));
#33545=CARTESIAN_POINT('',(17.9535710587063,37.2043320991532,41.0294657090004));
#33546=CARTESIAN_POINT('',(4.70570154376624,37.2043320991532,41.0294657090004));
#33547=CARTESIAN_POINT('Origin',(8.93978940303414,37.9543320991532,41.0294657090004));
#33548=CARTESIAN_POINT('',(2.61978940303414,37.2043320991532,41.0294657090004));
#33549=CARTESIAN_POINT('',(5.01073099165871,37.2043320991532,41.0294657090004));
#33550=CARTESIAN_POINT('',(2.61978940303414,34.9543320991532,41.0294657090004));
#33551=CARTESIAN_POINT('',(2.61978940303414,37.2043320991532,41.0294657090004));
#33552=CARTESIAN_POINT('',(2.61978940303414,34.9543320991532,41.0294657090004));
#33553=CARTESIAN_POINT('',(32.5397894030341,32.2543320991532,41.0294657090004));
#33554=CARTESIAN_POINT('',(32.8397894030341,32.2543320991532,41.0294657090004));
#33555=CARTESIAN_POINT('',(32.5397894030341,34.2543320991532,41.0294657090004));
#33556=CARTESIAN_POINT('',(32.5397894030341,43.9543320991532,41.0294657090004));
#33557=CARTESIAN_POINT('',(37.6397894030341,34.2543320991532,41.0294657090004));
#33558=CARTESIAN_POINT('',(0.939789403034137,34.2543320991532,41.0294657090004));
#33559=CARTESIAN_POINT('',(37.6397894030341,41.6543320991532,41.0294657090004));
#33560=CARTESIAN_POINT('',(37.6397894030341,43.9543320991532,41.0294657090004));
#33561=CARTESIAN_POINT('',(32.5397894030341,41.6543320991532,41.0294657090004));
#33562=CARTESIAN_POINT('',(0.939789403034137,41.6543320991532,41.0294657090004));
#33563=CARTESIAN_POINT('',(32.5397894030341,43.6543320991532,41.0294657090004));
#33564=CARTESIAN_POINT('',(32.5397894030341,43.9543320991532,41.0294657090004));
#33565=CARTESIAN_POINT('',(0.939789403034137,43.6543320991532,41.0294657090004));
#33566=CARTESIAN_POINT('',(2.61978940303414,40.9543320991532,41.0294657090004));
#33567=CARTESIAN_POINT('',(0.939789403034137,39.9843320991532,41.0294657090004));
#33568=CARTESIAN_POINT('',(2.61978940303414,38.7043320991532,41.0294657090004));
#33569=CARTESIAN_POINT('',(2.61978940303414,40.9543320991532,41.0294657090004));
#33570=CARTESIAN_POINT('',(4.70570154376623,38.7043320991532,41.0294657090004));
#33571=CARTESIAN_POINT('',(5.01073099165871,38.7043320991532,41.0294657090004));
#33572=CARTESIAN_POINT('Origin',(8.93978940303414,37.9543320991532,41.0294657090004));
#33573=CARTESIAN_POINT('Origin',(37.9397894030341,43.9543320991532,41.0294657090004));
#33574=CARTESIAN_POINT('',(37.9397894030341,41.9543320991532,35.0294657090004));
#33575=CARTESIAN_POINT('',(37.9397894030341,41.9543320991532,40.7294657090004));
#33576=CARTESIAN_POINT('',(37.9397894030341,41.9543320991532,41.0294657090004));
#33577=CARTESIAN_POINT('',(37.9397894030341,33.9543320991532,40.7294657090004));
#33578=CARTESIAN_POINT('',(37.9397894030341,43.9543320991532,40.7294657090004));
#33579=CARTESIAN_POINT('',(37.9397894030341,33.9543320991532,35.0294657090004));
#33580=CARTESIAN_POINT('',(37.9397894030341,33.9543320991532,41.0294657090004));
#33581=CARTESIAN_POINT('',(37.9397894030341,43.9543320991532,35.0294657090004));
#33582=CARTESIAN_POINT('Origin',(60.9397894030341,43.9543320991532,35.0294657090004));
#33583=CARTESIAN_POINT('',(43.0397894030341,33.9543320991532,35.0294657090004));
#33584=CARTESIAN_POINT('',(43.0397894030341,32.2543320991532,35.0294657090004));
#33585=CARTESIAN_POINT('',(43.0397894030341,43.9543320991532,35.0294657090004));
#33586=CARTESIAN_POINT('',(60.6397894030341,32.2543320991532,35.0294657090004));
#33587=CARTESIAN_POINT('',(60.9397894030341,32.2543320991532,35.0294657090004));
#33588=CARTESIAN_POINT('',(60.6397894030341,43.6543320991532,35.0294657090004));
#33589=CARTESIAN_POINT('',(60.6397894030341,43.9543320991532,35.0294657090004));
#33590=CARTESIAN_POINT('',(35.8397894030342,43.6543320991532,35.0294657090004));
#33591=CARTESIAN_POINT('',(60.9397894030341,43.6543320991532,35.0294657090004));
#33592=CARTESIAN_POINT('',(35.8397894030342,41.9543320991532,35.0294657090004));
#33593=CARTESIAN_POINT('',(35.8397894030342,41.9543320991532,35.0294657090004));
#33594=CARTESIAN_POINT('',(35.8397894030342,41.9543320991532,35.0294657090004));
#33595=CARTESIAN_POINT('',(60.9397894030341,33.9543320991532,35.0294657090004));
#33596=CARTESIAN_POINT('Origin',(30.9397894030341,43.9543320991532,35.0294657090004));
#33597=CARTESIAN_POINT('',(60.6397894030341,43.9543320991532,29.3294657090004));
#33598=CARTESIAN_POINT('',(1.23978940303414,43.9543320991532,29.3294657090004));
#33599=CARTESIAN_POINT('',(30.9397894030341,43.9543320991532,29.3294657090004));
#33600=CARTESIAN_POINT('',(1.23978940303414,43.9543320991532,40.7294657090004));
#33601=CARTESIAN_POINT('',(1.23978940303414,43.9543320991532,35.0294657090004));
#33602=CARTESIAN_POINT('',(32.5397894030341,43.9543320991532,40.7294657090004));
#33603=CARTESIAN_POINT('',(30.9397894030341,43.9543320991532,40.7294657090004));
#33604=CARTESIAN_POINT('',(32.5397894030341,43.9543320991532,38.0294657090004));
#33605=CARTESIAN_POINT('',(32.5397894030341,43.9543320991532,35.0294657090004));
#33606=CARTESIAN_POINT('',(35.8397894030342,43.9543320991532,34.7294657090004));
#33607=CARTESIAN_POINT('Origin',(35.8397894030341,43.9543320991532,38.0294657090004));
#33608=CARTESIAN_POINT('',(60.6397894030341,43.9543320991532,34.7294657090004));
#33609=CARTESIAN_POINT('',(30.9397894030341,43.9543320991532,34.7294657090004));
#33610=CARTESIAN_POINT('',(60.6397894030341,43.9543320991532,35.0294657090004));
#33611=CARTESIAN_POINT('Origin',(30.9397894030341,31.9543320991532,35.0294657090004));
#33612=CARTESIAN_POINT('',(60.6397894030341,31.9543320991532,29.3294657090004));
#33613=CARTESIAN_POINT('',(60.6397894030341,31.9543320991532,34.7294657090004));
#33614=CARTESIAN_POINT('',(60.6397894030341,31.9543320991532,35.0294657090004));
#33615=CARTESIAN_POINT('',(43.3397894030341,31.9543320991532,34.7294657090004));
#33616=CARTESIAN_POINT('',(43.0397894030341,31.9543320991532,34.7294657090004));
#33617=CARTESIAN_POINT('',(43.3397894030341,31.9543320991532,34.72672445582));
#33618=CARTESIAN_POINT('',(43.3397894030341,31.9543320991532,35.02672445582));
#33619=CARTESIAN_POINT('',(35.8397894030342,31.9543320991532,34.72672445582));
#33620=CARTESIAN_POINT('',(35.8397894030342,31.9543320991532,34.72672445582));
#33621=CARTESIAN_POINT('',(32.5397894030341,31.9543320991532,38.02672445582));
#33622=CARTESIAN_POINT('Origin',(35.8397894030341,31.9543320991532,38.02672445582));
#33623=CARTESIAN_POINT('',(32.5397894030341,31.9543320991532,40.7294657090004));
#33624=CARTESIAN_POINT('',(32.5397894030341,31.9543320991532,41.0294657090004));
#33625=CARTESIAN_POINT('',(1.23978940303414,31.9543320991532,40.7294657090004));
#33626=CARTESIAN_POINT('',(0.939789403034137,31.9543320991532,40.7294657090004));
#33627=CARTESIAN_POINT('',(1.23978940303414,31.9543320991532,29.3294657090004));
#33628=CARTESIAN_POINT('',(1.23978940303414,31.9543320991532,29.0294657090004));
#33629=CARTESIAN_POINT('',(60.9397894030341,31.9543320991532,29.3294657090004));
#33630=CARTESIAN_POINT('Origin',(8.93978940303414,37.9543320991532,41.0294657090004));
#33631=CARTESIAN_POINT('',(12.8688478144096,37.2043320991532,40.7294657090004));
#33632=CARTESIAN_POINT('',(12.8688478144096,37.2043320991532,29.3294657090004));
#33633=CARTESIAN_POINT('',(12.8688478144096,37.2043320991532,41.0294657090004));
#33634=CARTESIAN_POINT('',(5.01073099165871,37.2043320991532,29.3294657090004));
#33635=CARTESIAN_POINT('Origin',(8.93978940303414,37.9543320991532,29.3294657090004));
#33636=CARTESIAN_POINT('',(5.01073099165871,37.2043320991532,40.7294657090004));
#33637=CARTESIAN_POINT('',(5.01073099165871,37.2043320991532,41.0294657090004));
#33638=CARTESIAN_POINT('Origin',(8.93978940303414,37.9543320991532,40.7294657090004));
#33639=CARTESIAN_POINT('Origin',(17.9535710587063,37.2043320991532,41.0294657090004));
#33640=CARTESIAN_POINT('Ctrl Pts',(13.1738772623021,37.2043320991532,29.0294657090004));
#33641=CARTESIAN_POINT('Ctrl Pts',(13.0722597271638,37.2043320991532,29.1295256094231));
#33642=CARTESIAN_POINT('Ctrl Pts',(12.9705877024409,37.2043320991532,29.2295302182899));
#33643=CARTESIAN_POINT('Ctrl Pts',(12.8688478144096,37.2043320991532,29.3294657090004));
#33644=CARTESIAN_POINT('Ctrl Pts',(12.8688478144096,37.2043320991532,40.7294657090004));
#33645=CARTESIAN_POINT('Ctrl Pts',(12.9705877024409,37.2043320991532,40.8294011997109));
#33646=CARTESIAN_POINT('Ctrl Pts',(13.0722597271638,37.2043320991532,40.9294058085777));
#33647=CARTESIAN_POINT('Ctrl Pts',(13.173877262302,37.2043320991532,41.0294657090004));
#33648=CARTESIAN_POINT('Origin',(19.1460502915689,38.7043320991532,41.0294657090004));
#33649=CARTESIAN_POINT('',(12.8688478144096,38.7043320991532,40.7294657090004));
#33650=CARTESIAN_POINT('',(12.8688478144096,38.7043320991532,29.3294657090004));
#33651=CARTESIAN_POINT('',(12.8688478144096,38.7043320991532,41.0294657090004));
#33652=CARTESIAN_POINT('Ctrl Pts',(12.8688478144096,38.7043320991532,29.3294657090004));
#33653=CARTESIAN_POINT('Ctrl Pts',(12.9705877024409,38.7043320991532,29.2295302182899));
#33654=CARTESIAN_POINT('Ctrl Pts',(13.0722597271638,38.7043320991532,29.1295256094231));
#33655=CARTESIAN_POINT('Ctrl Pts',(13.1738772623021,38.7043320991532,29.0294657090004));
#33656=CARTESIAN_POINT('Ctrl Pts',(13.173877262302,38.7043320991532,41.0294657090004));
#33657=CARTESIAN_POINT('Ctrl Pts',(13.0722597271638,38.7043320991532,40.9294058085776));
#33658=CARTESIAN_POINT('Ctrl Pts',(12.9705877024409,38.7043320991532,40.8294011997109));
#33659=CARTESIAN_POINT('Ctrl Pts',(12.8688478144096,38.7043320991532,40.7294657090004));
#33660=CARTESIAN_POINT('Origin',(8.93978940303414,37.9543320991532,41.0294657090004));
#33661=CARTESIAN_POINT('',(5.01073099165871,38.7043320991532,40.7294657090004));
#33662=CARTESIAN_POINT('',(5.01073099165871,38.7043320991532,29.3294657090004));
#33663=CARTESIAN_POINT('',(5.01073099165871,38.7043320991532,41.0294657090004));
#33664=CARTESIAN_POINT('Origin',(8.93978940303414,37.9543320991532,29.3294657090004));
#33665=CARTESIAN_POINT('Origin',(8.93978940303414,37.9543320991532,40.7294657090004));
#33666=CARTESIAN_POINT('Origin',(5.01073099165871,38.7043320991532,41.0294657090004));
#33667=CARTESIAN_POINT('Ctrl Pts',(4.70570154376622,38.7043320991532,29.0294657090004));
#33668=CARTESIAN_POINT('Ctrl Pts',(4.80731907890448,38.7043320991532,29.1295256094231));
#33669=CARTESIAN_POINT('Ctrl Pts',(4.90899110362736,38.7043320991532,29.2295302182899));
#33670=CARTESIAN_POINT('Ctrl Pts',(5.01073099165871,38.7043320991532,29.3294657090004));
#33671=CARTESIAN_POINT('Ctrl Pts',(5.01073099165871,38.7043320991532,40.7294657090004));
#33672=CARTESIAN_POINT('Ctrl Pts',(4.90899110362737,38.7043320991532,40.8294011997109));
#33673=CARTESIAN_POINT('Ctrl Pts',(4.80731907890448,38.7043320991532,40.9294058085776));
#33674=CARTESIAN_POINT('Ctrl Pts',(4.70570154376623,38.7043320991532,41.0294657090004));
#33675=CARTESIAN_POINT('',(2.61978940303414,38.7043320991532,41.0294657090004));
#33676=CARTESIAN_POINT('Origin',(2.61978940303414,40.9543320991532,41.0294657090004));
#33677=CARTESIAN_POINT('',(2.61978940303414,40.9543320991532,41.0294657090004));
#33678=CARTESIAN_POINT('Origin',(0.939789403034137,39.9843320991532,41.0294657090004));
#33679=CARTESIAN_POINT('Origin',(2.61978940303414,34.9543320991532,41.0294657090004));
#33680=CARTESIAN_POINT('',(2.61978940303414,34.9543320991532,41.0294657090004));
#33681=CARTESIAN_POINT('Origin',(2.61978940303414,37.2043320991532,41.0294657090004));
#33682=CARTESIAN_POINT('',(2.61978940303414,37.2043320991532,41.0294657090004));
#33683=CARTESIAN_POINT('Origin',(5.01073099165871,37.2043320991532,41.0294657090004));
#33684=CARTESIAN_POINT('Ctrl Pts',(5.01073099165871,37.2043320991532,29.3294657090004));
#33685=CARTESIAN_POINT('Ctrl Pts',(4.90899110362736,37.2043320991532,29.2295302182899));
#33686=CARTESIAN_POINT('Ctrl Pts',(4.80731907890448,37.2043320991532,29.1295256094231));
#33687=CARTESIAN_POINT('Ctrl Pts',(4.70570154376622,37.2043320991532,29.0294657090004));
#33688=CARTESIAN_POINT('Ctrl Pts',(4.70570154376624,37.2043320991532,41.0294657090004));
#33689=CARTESIAN_POINT('Ctrl Pts',(4.80731907890449,37.2043320991532,40.9294058085777));
#33690=CARTESIAN_POINT('Ctrl Pts',(4.90899110362737,37.2043320991532,40.8294011997109));
#33691=CARTESIAN_POINT('Ctrl Pts',(5.01073099165871,37.2043320991532,40.7294657090004));
#33692=CARTESIAN_POINT('Origin',(35.8397894030341,33.9543320991532,38.02672445582));
#33693=CARTESIAN_POINT('',(32.8397894030341,33.9543320991532,40.7294657090004));
#33694=CARTESIAN_POINT('',(35.8397894030341,33.9543320991532,40.7294657090004));
#33695=CARTESIAN_POINT('',(32.8397894030341,33.9543320991532,38.02672445582));
#33696=CARTESIAN_POINT('',(32.8397894030341,33.9543320991532,47.0322069621808));
#33697=CARTESIAN_POINT('',(35.8397894030342,33.9543320991532,35.02672445582));
#33698=CARTESIAN_POINT('Origin',(35.8397894030341,33.9543320991532,38.02672445582));
#33699=CARTESIAN_POINT('',(43.0397894030341,33.9543320991532,35.02672445582));
#33700=CARTESIAN_POINT('',(43.0397894030341,33.9543320991532,35.02672445582));
#33701=CARTESIAN_POINT('',(43.0397894030341,33.9543320991532,47.0322069621808));
#33702=CARTESIAN_POINT('Origin',(43.0397894030341,33.9543320991532,47.0322069621808));
#33703=CARTESIAN_POINT('',(43.0397894030341,32.2543320991532,35.02672445582));
#33704=CARTESIAN_POINT('',(43.0397894030341,33.9543320991532,35.02672445582));
#33705=CARTESIAN_POINT('',(43.0397894030341,32.2543320991532,35.0294657090004));
#33706=CARTESIAN_POINT('Origin',(32.8397894030341,33.9543320991532,47.0322069621808));
#33707=CARTESIAN_POINT('',(32.8397894030341,32.2543320991532,40.7294657090004));
#33708=CARTESIAN_POINT('',(32.8397894030341,33.9543320991532,40.7294657090004));
#33709=CARTESIAN_POINT('',(32.8397894030341,32.2543320991532,38.02672445582));
#33710=CARTESIAN_POINT('',(32.8397894030341,32.2543320991532,38.02672445582));
#33711=CARTESIAN_POINT('',(32.8397894030341,33.9543320991532,38.02672445582));
#33712=CARTESIAN_POINT('Origin',(43.0397894030341,33.9543320991532,35.02672445582));
#33713=CARTESIAN_POINT('',(35.8397894030342,32.2543320991532,35.02672445582));
#33714=CARTESIAN_POINT('',(35.8397894030342,33.9543320991532,35.02672445582));
#33715=CARTESIAN_POINT('',(43.0397894030341,32.2543320991532,35.02672445582));
#33716=CARTESIAN_POINT('Origin',(35.8397894030341,33.9543320991532,38.02672445582));
#33717=CARTESIAN_POINT('Origin',(35.8397894030341,32.2543320991532,38.02672445582));
#33718=CARTESIAN_POINT('Origin',(35.8397894030341,41.9543320991532,38.0294657090004));
#33719=CARTESIAN_POINT('',(32.8397894030341,41.9543320991532,38.0294657090004));
#33720=CARTESIAN_POINT('',(32.8397894030341,41.9543320991532,40.7294657090004));
#33721=CARTESIAN_POINT('',(32.8397894030341,41.9543320991532,47.0294657090004));
#33722=CARTESIAN_POINT('',(35.8397894030341,41.9543320991532,40.7294657090004));
#33723=CARTESIAN_POINT('Origin',(35.8397894030341,41.9543320991532,38.0294657090004));
#33724=CARTESIAN_POINT('Origin',(32.8397894030341,41.9543320991532,47.0294657090004));
#33725=CARTESIAN_POINT('',(32.8397894030341,43.6543320991532,38.0294657090004));
#33726=CARTESIAN_POINT('',(32.8397894030341,43.6543320991532,40.7294657090004));
#33727=CARTESIAN_POINT('',(32.8397894030341,43.6543320991532,47.0294657090004));
#33728=CARTESIAN_POINT('',(32.8397894030341,41.9543320991532,40.7294657090004));
#33729=CARTESIAN_POINT('',(32.8397894030341,41.9543320991532,38.0294657090004));
#33730=CARTESIAN_POINT('Origin',(35.8397894030341,41.9543320991532,38.0294657090004));
#33731=CARTESIAN_POINT('Origin',(35.8397894030341,43.6543320991532,38.0294657090004));
#33732=CARTESIAN_POINT('Origin',(30.9397894030341,43.6543320991532,40.7294657090004));
#33733=CARTESIAN_POINT('Origin',(32.5397894030341,43.6543320991532,40.7294657090004));
#33734=CARTESIAN_POINT('Origin',(1.23978940303386,43.6543320991535,40.7294657090006));
#33735=CARTESIAN_POINT('Origin',(1.23978940303414,43.6543320991532,35.0294657090004));
#33736=CARTESIAN_POINT('Origin',(1.23978940303469,43.6543320991527,29.3294657090009));
#33737=CARTESIAN_POINT('Origin',(32.5397894030341,43.6543320991532,47.0294657090004));
#33738=CARTESIAN_POINT('Origin',(32.5397894030341,43.6543320991532,40.7294657090004));
#33739=CARTESIAN_POINT('Origin',(32.5397894030341,43.6543320991532,38.0294657090004));
#33740=CARTESIAN_POINT('Origin',(30.9397894030341,43.6543320991532,29.3294657090004));
#33741=CARTESIAN_POINT('Origin',(60.6397894030341,43.6543320991532,29.3294657090004));
#33742=CARTESIAN_POINT('Origin',(0.939789403034137,32.2543320991532,40.7294657090004));
#33743=CARTESIAN_POINT('Origin',(32.5397894030341,32.2543320991532,40.7294657090004));
#33744=CARTESIAN_POINT('Origin',(1.23978940303371,32.2543320991528,40.7294657090008));
#33745=CARTESIAN_POINT('Origin',(35.8397894030341,43.6543320991532,38.0294657090004));
#33746=CARTESIAN_POINT('Origin',(35.8397894030342,43.6543320991532,34.7294657090004));
#33747=CARTESIAN_POINT('Origin',(60.6397894030341,43.6543320991532,29.3294657090004));
#33748=CARTESIAN_POINT('Origin',(60.6397894030341,43.6543320991532,29.3294657090004));
#33749=CARTESIAN_POINT('Origin',(60.6397894030341,43.6543320991532,29.3294657090004));
#33750=CARTESIAN_POINT('Origin',(1.23978940303414,32.2543320991532,41.0294657090004));
#33751=CARTESIAN_POINT('Origin',(1.23978940303447,32.2543320991536,29.3294657090007));
#33752=CARTESIAN_POINT('Origin',(32.5397894030341,32.2543320991532,47.0322069621808));
#33753=CARTESIAN_POINT('Origin',(32.5397894030341,32.2543320991532,40.7294657090004));
#33754=CARTESIAN_POINT('Origin',(32.5397894030341,32.2543320991532,38.02672445582));
#33755=CARTESIAN_POINT('Origin',(30.9397894030341,43.6543320991532,34.7294657090004));
#33756=CARTESIAN_POINT('Origin',(60.6397894030341,43.6543320991532,34.7294657090004));
#33757=CARTESIAN_POINT('Origin',(60.6397894030341,43.6543320991532,35.0294657090004));
#33758=CARTESIAN_POINT('Origin',(60.6397894030341,43.6543320991532,34.7294657090004));
#33759=CARTESIAN_POINT('Origin',(60.6397894030341,43.9543320991532,29.3294657090004));
#33760=CARTESIAN_POINT('Origin',(60.6397894030341,32.2543320991532,29.3294657090004));
#33761=CARTESIAN_POINT('Origin',(0.939789403034137,32.2543320991532,29.3294657090004));
#33762=CARTESIAN_POINT('Origin',(60.6397894030341,32.2543320991532,29.3294657090004));
#33763=CARTESIAN_POINT('Origin',(35.8397894030341,32.2543320991532,38.02672445582));
#33764=CARTESIAN_POINT('Origin',(35.8397894030342,32.2543320991532,34.72672445582));
#33765=CARTESIAN_POINT('Origin',(60.6397894030341,43.6543320991532,34.7294657090004));
#33766=CARTESIAN_POINT('Origin',(60.6397894030341,43.6543320991532,34.7294657090004));
#33767=CARTESIAN_POINT('Origin',(60.6397894030341,32.2543320991532,29.3294657090004));
#33768=CARTESIAN_POINT('Origin',(60.6397894030341,32.2543320991532,29.3294657090004));
#33769=CARTESIAN_POINT('Origin',(43.0397894030341,32.2543320991532,34.72672445582));
#33770=CARTESIAN_POINT('Origin',(43.3397894030341,32.2543320991531,34.72672445582));
#33771=CARTESIAN_POINT('Origin',(60.6397894030341,43.9543320991532,34.7294657090004));
#33772=CARTESIAN_POINT('Origin',(60.6397894030341,32.2543320991532,34.7294657090004));
#33773=CARTESIAN_POINT('Origin',(60.6397894030341,32.2543320991532,35.0294657090004));
#33774=CARTESIAN_POINT('Origin',(60.6397894030341,32.2543320991532,34.7294657090004));
#33775=CARTESIAN_POINT('Origin',(43.3397894030341,32.2543320991532,47.0322069621808));
#33776=CARTESIAN_POINT('Origin',(43.3397894030341,32.2543320991532,34.7294657090004));
#33777=CARTESIAN_POINT('Origin',(60.6397894030341,32.2543320991532,34.7294657090004));
#33778=CARTESIAN_POINT('Origin',(60.6397894030341,32.2543320991532,34.7294657090004));
#33779=CARTESIAN_POINT('Origin',(60.9397894030341,32.2543320991532,34.7294657090004));
#33780=CARTESIAN_POINT('Origin',(32.5397894030341,43.6543320991532,40.7294657090004));
#33781=CARTESIAN_POINT('Origin',(32.5397894030341,43.6543320991532,40.7294657090004));
#33782=CARTESIAN_POINT('Origin',(32.5397894030341,43.9543320991532,40.7294657090004));
#33783=CARTESIAN_POINT('Origin',(32.5397894030357,41.6543320991548,40.7294657090019));
#33784=CARTESIAN_POINT('Origin',(0.939789403034137,41.6543320991532,40.7294657090004));
#33785=CARTESIAN_POINT('Origin',(37.6397894030353,41.6543320991544,40.7294657090015));
#33786=CARTESIAN_POINT('Origin',(37.6397894030341,43.9543320991532,40.7294657090004));
#33787=CARTESIAN_POINT('Origin',(37.6397894030347,34.2543320991526,40.729465709001));
#33788=CARTESIAN_POINT('Origin',(0.939789403034137,34.2543320991532,40.7294657090004));
#33789=CARTESIAN_POINT('Origin',(32.5397894030352,34.2543320991522,40.7294657090014));
#33790=CARTESIAN_POINT('Origin',(32.5397894030341,43.9543320991532,40.7294657090004));
#33791=CARTESIAN_POINT('Origin',(32.5397894030341,32.2543320991532,40.7294657090004));
#33792=CARTESIAN_POINT('Origin',(32.5397894030341,32.2543320991532,40.7294657090004));
#33793=CARTESIAN_POINT('Origin',(8.93978940303414,37.9543320991532,29.3294657090004));
#33794=CARTESIAN_POINT('Origin',(8.93978940303414,37.9543320991532,29.3294657090004));
#33795=CARTESIAN_POINT('Origin',(8.93978940303414,37.9543320991532,41.0294657090004));
#33796=CARTESIAN_POINT('Origin',(8.93978940303414,37.9543320991532,41.0294657090004));
#33797=CARTESIAN_POINT('Origin',(35.9397894030337,32.0543320991536,38.5294657090004));
#33798=CARTESIAN_POINT('',(34.8397894030337,31.9543320991536,38.5294657090004));
#33799=CARTESIAN_POINT('Origin',(35.9397894030337,31.9543320991536,38.5294657090004));
#33800=CARTESIAN_POINT('',(34.7397894030337,32.0543320991536,38.5294657090004));
#33801=CARTESIAN_POINT('Origin',(34.8397894030337,32.0543320991536,38.5294657090004));
#33802=CARTESIAN_POINT('',(37.1397894030337,32.0543320991536,38.5294657090004));
#33803=CARTESIAN_POINT('Origin',(35.9397894030337,32.0543320991536,38.5294657090004));
#33804=CARTESIAN_POINT('Origin',(35.9397894030337,32.0543320991536,38.5294657090004));
#33805=CARTESIAN_POINT('Origin',(35.9397894030336,43.8543320991536,38.5294657090005));
#33806=CARTESIAN_POINT('',(37.1397894030336,43.8543320991536,38.5294657090004));
#33807=CARTESIAN_POINT('',(34.7397894030336,43.8543320991536,38.5294657090005));
#33808=CARTESIAN_POINT('Origin',(35.9397894030336,43.8543320991536,38.5294657090005));
#33809=CARTESIAN_POINT('Origin',(35.9397894030336,43.8543320991536,38.5294657090005));
#33810=CARTESIAN_POINT('',(34.8397894030336,43.9543320991536,38.5294657090005));
#33811=CARTESIAN_POINT('Origin',(34.8397894030336,43.8543320991536,38.5294657090005));
#33812=CARTESIAN_POINT('Origin',(35.9397894030336,43.9543320991536,38.5294657090005));
#33813=CARTESIAN_POINT('Origin',(35.9397894030337,31.9543320991536,38.5294657090004));
#33814=CARTESIAN_POINT('',(37.1397894030337,31.9543320991536,38.5294657090004));
#33815=CARTESIAN_POINT('Origin',(35.9397894030337,31.9543320991536,38.5294657090004));
#33816=CARTESIAN_POINT('Origin',(35.9397894030336,43.9543320991536,38.5294657090005));
#33817=CARTESIAN_POINT('Origin',(71.9308774154808,37.9543320991532,39.3304548976388));
#33818=CARTESIAN_POINT('',(66.9321151915299,35.4543320991532,39.2192063992168));
#33819=CARTESIAN_POINT('Origin',(66.9321151915299,37.9543320991532,39.2192063992168));
#33820=CARTESIAN_POINT('',(71.9308774154808,35.4543320991532,39.3304548976388));
#33821=CARTESIAN_POINT('',(71.9308774154808,35.4543320991532,39.3304548976388));
#33822=CARTESIAN_POINT('Origin',(71.9308774154808,37.9543320991532,39.3304548976388));
#33823=CARTESIAN_POINT('Origin',(66.9321151915299,37.9543320991532,39.2192063992168));
#33824=CARTESIAN_POINT('',(61.000349621842,37.9543320991532,36.0864508667399));
#33825=CARTESIAN_POINT('',(60.8668514237356,37.9543320991532,42.084965535481));
#33826=CARTESIAN_POINT('Origin',(60.9336005227888,37.9543320991532,39.0857082011104));
#33827=CARTESIAN_POINT('',(60.9336005227888,34.9543320991532,39.0857082011104));
#33828=CARTESIAN_POINT('Origin',(60.9336005227888,37.9543320991532,39.0857082011104));
#33829=CARTESIAN_POINT('',(66.9321151915299,34.9543320991532,39.2192063992168));
#33830=CARTESIAN_POINT('',(66.9321151915299,34.9543320991532,39.2192063992168));
#33831=CARTESIAN_POINT('Origin',(66.9321151915299,37.9543320991532,39.2192063992168));
#33832=CARTESIAN_POINT('Origin',(60.9336005227888,37.9543320991532,39.0857082011104));
#33833=CARTESIAN_POINT('Origin',(43.4824321383293,37.9543320991532,36.6968335670531));
#33834=CARTESIAN_POINT('',(39.233484247971,37.9543320991532,36.6022723433944));
#33835=CARTESIAN_POINT('Origin',(43.4824321383293,37.9543320991532,36.6968335670531));
#33836=CARTESIAN_POINT('',(39.122235749549,37.9543320991532,41.6010345673453));
#33837=CARTESIAN_POINT('',(39.233484247971,37.9543320991532,36.6022723433944));
#33838=CARTESIAN_POINT('Origin',(43.3711836399073,37.9543320991532,41.695595791004));
#33839=CARTESIAN_POINT('Origin',(35.9397894030341,43.9543320991532,38.5294657090004));
#33840=CARTESIAN_POINT('',(37.1394923367823,33.9543320991532,38.5561653486217));
#33841=CARTESIAN_POINT('Origin',(35.9397894030341,33.9543320991532,38.5294657090004));
#33842=CARTESIAN_POINT('',(37.1394923367823,31.9543320991532,38.5561653486217));
#33843=CARTESIAN_POINT('',(37.1394923367823,43.9543320991532,38.5561653486217));
#33844=CARTESIAN_POINT('Origin',(35.9397894030341,31.9543320991532,38.5294657090004));
#33845=CARTESIAN_POINT('Origin',(35.9397894030341,43.9543320991532,38.5294657090004));
#33846=CARTESIAN_POINT('',(37.1394923367823,43.9543320991532,38.5561653486217));
#33847=CARTESIAN_POINT('Origin',(35.9397894030341,43.9543320991532,38.5294657090004));
#33848=CARTESIAN_POINT('',(37.1394923367823,41.9543320991532,38.5561653486217));
#33849=CARTESIAN_POINT('',(37.1394923367823,43.9543320991532,38.5561653486217));
#33850=CARTESIAN_POINT('Origin',(35.9397894030341,41.9543320991532,38.5294657090004));
#33851=CARTESIAN_POINT('Origin',(43.5046818380137,37.9543320991532,35.6970811222629));
#33852=CARTESIAN_POINT('',(41.5051769484333,37.9543320991532,35.6525817228941));
#33853=CARTESIAN_POINT('Origin',(43.5046818380137,37.9543320991532,35.6970811222629));
#33854=CARTESIAN_POINT('',(41.4829272487489,37.9543320991532,36.6523341676843));
#33855=CARTESIAN_POINT('',(41.5051769484333,37.9543320991532,35.6525817228941));
#33856=CARTESIAN_POINT('Origin',(43.4824321383293,37.9543320991532,36.6968335670531));
#33857=CARTESIAN_POINT('Origin',(60.8668514237356,43.9543320991532,42.084965535481));
#33858=CARTESIAN_POINT('',(61.000349621842,43.9543320991532,36.0864508667399));
#33859=CARTESIAN_POINT('',(61.000349621842,43.9543320991532,36.0864508667399));
#33860=CARTESIAN_POINT('',(60.8668514237356,43.9543320991532,42.084965535481));
#33861=CARTESIAN_POINT('',(60.8668514237356,43.9543320991532,42.084965535481));
#33862=CARTESIAN_POINT('',(60.8668514237356,43.9543320991532,42.084965535481));
#33863=CARTESIAN_POINT('Origin',(34.4735352853754,43.9543320991532,36.9964624922886));
#33864=CARTESIAN_POINT('',(34.506909834902,43.9543320991532,35.4968338251033));
#33865=CARTESIAN_POINT('',(34.506909834902,41.9543320991532,35.4968338251033));
#33866=CARTESIAN_POINT('',(34.506909834902,43.9543320991532,35.4968338251033));
#33867=CARTESIAN_POINT('',(32.9739066181901,41.9543320991532,36.963087942762));
#33868=CARTESIAN_POINT('Origin',(34.4735352853754,41.9543320991532,36.9964624922886));
#33869=CARTESIAN_POINT('',(32.9739066181901,43.9543320991532,36.963087942762));
#33870=CARTESIAN_POINT('',(32.9739066181901,43.9543320991532,36.963087942762));
#33871=CARTESIAN_POINT('Origin',(34.4735352853754,43.9543320991532,36.9964624922886));
#33872=CARTESIAN_POINT('Origin',(32.8737829696103,43.9543320991532,41.4619739443178));
#33873=CARTESIAN_POINT('',(32.8737829696103,41.9543320991532,41.4619739443178));
#33874=CARTESIAN_POINT('',(32.8737829696103,41.9543320991532,41.4619739443178));
#33875=CARTESIAN_POINT('',(32.8737829696103,43.9543320991532,41.4619739443178));
#33876=CARTESIAN_POINT('',(32.8737829696103,43.9543320991532,41.4619739443178));
#33877=CARTESIAN_POINT('',(32.8737829696103,43.9543320991532,41.4619739443178));
#33878=CARTESIAN_POINT('Origin',(34.4735352853754,43.9543320991532,36.9964624922886));
#33879=CARTESIAN_POINT('',(34.506909834902,43.9543320991532,35.4968338251033));
#33880=CARTESIAN_POINT('',(32.8737829696103,43.9543320991532,41.4619739443178));
#33881=CARTESIAN_POINT('Origin',(34.4735352853754,31.9543320991532,36.9964624922886));
#33882=CARTESIAN_POINT('',(60.8668514237356,31.9543320991532,42.084965535481));
#33883=CARTESIAN_POINT('',(61.000349621842,31.9543320991532,36.0864508667399));
#33884=CARTESIAN_POINT('',(60.8668514237356,31.9543320991532,42.084965535481));
#33885=CARTESIAN_POINT('',(32.8737829696103,31.9543320991532,41.4619739443178));
#33886=CARTESIAN_POINT('',(32.8737829696103,31.9543320991532,41.4619739443178));
#33887=CARTESIAN_POINT('',(32.9739066181901,31.9543320991532,36.963087942762));
#33888=CARTESIAN_POINT('',(32.8737829696103,31.9543320991532,41.4619739443178));
#33889=CARTESIAN_POINT('',(34.506909834902,31.9543320991532,35.4968338251033));
#33890=CARTESIAN_POINT('Origin',(34.4735352853754,31.9543320991532,36.9964624922886));
#33891=CARTESIAN_POINT('',(34.506909834902,31.9543320991532,35.4968338251033));
#33892=CARTESIAN_POINT('Origin',(60.8668514237356,43.9543320991532,42.084965535481));
#33893=CARTESIAN_POINT('',(60.8668514237356,43.9543320991532,42.084965535481));
#33894=CARTESIAN_POINT('',(61.000349621842,43.9543320991532,36.0864508667399));
#33895=CARTESIAN_POINT('Origin',(34.506909834902,43.9543320991532,35.4968338251033));
#33896=CARTESIAN_POINT('',(38.5059196140628,41.9543320991532,35.5858326238409));
#33897=CARTESIAN_POINT('',(38.5059196140628,33.9543320991532,35.5858326238409));
#33898=CARTESIAN_POINT('',(38.5059196140628,33.9543320991532,35.5858326238409));
#33899=CARTESIAN_POINT('',(30.5079000557413,41.9543320991532,35.4078350263657));
#33900=CARTESIAN_POINT('',(34.506909834902,33.9543320991532,35.4968338251033));
#33901=CARTESIAN_POINT('',(34.506909834902,43.9543320991532,35.4968338251033));
#33902=CARTESIAN_POINT('',(30.5079000557413,33.9543320991532,35.4078350263657));
#33903=CARTESIAN_POINT('Origin',(34.4735352853754,43.9543320991532,36.9964624922886));
#33904=CARTESIAN_POINT('',(32.9739066181901,33.9543320991532,36.963087942762));
#33905=CARTESIAN_POINT('',(32.9739066181901,43.9543320991532,36.963087942762));
#33906=CARTESIAN_POINT('Origin',(34.4735352853754,33.9543320991532,36.9964624922886));
#33907=CARTESIAN_POINT('Origin',(32.8737829696103,43.9543320991532,41.4619739443178));
#33908=CARTESIAN_POINT('',(32.8737829696103,33.9543320991532,41.4619739443178));
#33909=CARTESIAN_POINT('',(32.8737829696103,43.9543320991532,41.4619739443178));
#33910=CARTESIAN_POINT('',(32.8737829696103,33.9543320991532,41.4619739443178));
#33911=CARTESIAN_POINT('Origin',(32.8737829696103,43.9543320991532,41.4619739443178));
#33912=CARTESIAN_POINT('',(38.3724214159564,41.9543320991532,41.584347292582));
#33913=CARTESIAN_POINT('',(30.3744018576349,41.9543320991532,41.4063496951068));
#33914=CARTESIAN_POINT('',(38.3724214159564,33.9543320991532,41.584347292582));
#33915=CARTESIAN_POINT('',(38.3724214159564,33.9543320991532,41.584347292582));
#33916=CARTESIAN_POINT('',(30.3744018576349,33.9543320991532,41.4063496951068));
#33917=CARTESIAN_POINT('Origin',(30.3744018576349,41.9543320991532,41.4063496951068));
#33918=CARTESIAN_POINT('',(38.3724214159564,41.9543320991532,41.584347292582));
#33919=CARTESIAN_POINT('Origin',(30.3744018576349,33.9543320991532,41.4063496951068));
#33920=CARTESIAN_POINT('',(38.3724214159564,33.9543320991532,41.584347292582));
#33921=CARTESIAN_POINT('Origin',(38.3724214159564,33.9543320991532,41.584347292582));
#33922=CARTESIAN_POINT('Origin',(43.4824321383293,37.9543320991532,36.6968335670531));
#33923=CARTESIAN_POINT('Origin',(66.9321151915299,37.9543320991532,39.2192063992168));
#33924=CARTESIAN_POINT('Origin',(71.9308774154808,37.9543320991532,39.3304548976388));
#33925=CARTESIAN_POINT('Origin',(83.7526213271442,37.9543320991532,39.5935502800518));
#33926=CARTESIAN_POINT('',(66.9872301765546,38.2918510578248,36.7427082080277));
#33927=CARTESIAN_POINT('Origin',(66.93211519153,37.9543320991532,39.2192063992168));
#33928=CARTESIAN_POINT('',(71.9859924005056,38.2918510578248,36.8539567064497));
#33929=CARTESIAN_POINT('',(83.8077363121688,38.2918510578248,37.1170520888627));
#33930=CARTESIAN_POINT('Origin',(71.930877415481,37.9543320991532,39.3304548976388));
#33931=CARTESIAN_POINT('Origin',(71.829881909202,37.9543320991532,39.3282072215307));
#33932=CARTESIAN_POINT('',(71.8133605791719,43.4039772078075,40.0705651105397));
#33933=CARTESIAN_POINT('',(71.8464032392321,32.5046869904988,38.5858493325217));
#33934=CARTESIAN_POINT('Origin',(71.829881909202,37.9543320991532,39.3282072215307));
#33935=CARTESIAN_POINT('Origin',(71.930877415481,37.9543320991532,39.3304548976388));
#33936=CARTESIAN_POINT('Origin',(54.9397894030341,37.9543320991532,23.5294657090004));
#33937=CARTESIAN_POINT('',(57.4397894030341,37.9543320991532,23.0294657090004));
#33938=CARTESIAN_POINT('Origin',(54.9397894030341,37.9543320991532,23.0294657090004));
#33939=CARTESIAN_POINT('',(56.9397894030341,37.9543320991532,23.5294657090004));
#33940=CARTESIAN_POINT('Origin',(57.4397894030341,37.9543320991532,23.5294657090004));
#33941=CARTESIAN_POINT('Origin',(54.9397894030341,37.9543320991532,23.5294657090004));
#33942=CARTESIAN_POINT('Origin',(54.9397894030341,37.9543320991532,34.6394657090004));
#33943=CARTESIAN_POINT('',(54.9397894030341,35.9561834064188,34.6413170162659));
#33944=CARTESIAN_POINT('',(56.9379380957686,37.9543320991532,34.6413170162659));
#33945=CARTESIAN_POINT('Origin',(54.9397894030341,37.9543320991532,34.6413170162659));
#33946=CARTESIAN_POINT('Origin',(54.9397894030341,37.9543320991532,34.6413170162659));
#33947=CARTESIAN_POINT('',(56.5497894030341,37.9543320991532,35.0294657090004));
#33948=CARTESIAN_POINT('',(56.9397894030341,37.9543320991532,34.6394657090004));
#33949=CARTESIAN_POINT('Origin',(54.9397894030341,37.9543320991532,35.0294657090004));
#33950=CARTESIAN_POINT('Origin',(54.9397894030341,37.9543320991532,34.369532375667));
#33951=CARTESIAN_POINT('',(56.9397894030342,37.9543320991532,34.0964514357652));
#33952=CARTESIAN_POINT('',(54.9397894030341,39.9543320991532,34.0964514357652));
#33953=CARTESIAN_POINT('Origin',(54.9397894030341,37.9543320991532,34.0964514357652));
#33954=CARTESIAN_POINT('Origin',(54.9397894030341,37.9543320991532,34.0964514357652));
#33955=CARTESIAN_POINT('',(54.9397894030341,39.5643320991532,34.369532375667));
#33956=CARTESIAN_POINT('',(54.9397894030341,39.5643320991532,34.369532375667));
#33957=CARTESIAN_POINT('',(54.9397894030341,36.3443320991532,34.369532375667));
#33958=CARTESIAN_POINT('Origin',(54.9397894030341,37.9543320991532,34.369532375667));
#33959=CARTESIAN_POINT('Origin',(54.9397894030341,37.9543320991532,34.369532375667));
#33960=CARTESIAN_POINT('Origin',(54.9397894030341,37.9543320991532,34.6426133155688));
#33961=CARTESIAN_POINT('',(54.9397894030341,35.9543320991532,34.6426133155688));
#33962=CARTESIAN_POINT('Origin',(54.9397894030341,37.9543320991532,8.12867690713751));
#33963=CARTESIAN_POINT('',(54.9397894030341,35.9543320991532,33.9826799822355));
#33964=CARTESIAN_POINT('',(56.9397894030342,37.9543320991532,33.9826799822355));
#33965=CARTESIAN_POINT('Origin',(54.9397894030341,37.9543320991532,33.9826799822355));
#33966=CARTESIAN_POINT('Origin',(54.9397894030341,37.9543320991532,33.9826799822355));
#33967=CARTESIAN_POINT('',(56.9397894030341,37.9543320991532,8.12867690713751));
#33968=CARTESIAN_POINT('Origin',(54.9397894030341,37.9543320991532,33.7095990423337));
#33969=CARTESIAN_POINT('',(56.9397894030342,37.9543320991532,33.4365181024319));
#33970=CARTESIAN_POINT('',(54.9397894030341,39.9543320991532,33.4365181024319));
#33971=CARTESIAN_POINT('Origin',(54.9397894030341,37.9543320991532,33.4365181024319));
#33972=CARTESIAN_POINT('Origin',(54.9397894030341,37.9543320991532,33.4365181024319));
#33973=CARTESIAN_POINT('',(54.9397894030341,39.5643320991532,33.7095990423337));
#33974=CARTESIAN_POINT('',(54.9397894030341,39.5643320991532,33.7095990423337));
#33975=CARTESIAN_POINT('',(54.9397894030341,36.3443320991532,33.7095990423337));
#33976=CARTESIAN_POINT('Origin',(54.9397894030341,37.9543320991532,33.7095990423337));
#33977=CARTESIAN_POINT('Origin',(54.9397894030341,37.9543320991532,33.7095990423337));
#33978=CARTESIAN_POINT('Origin',(54.9397894030341,37.9543320991532,33.9826799822355));
#33979=CARTESIAN_POINT('',(54.9397894030341,35.9543320991532,33.9826799822355));
#33980=CARTESIAN_POINT('Origin',(54.9397894030341,37.9543320991532,8.12867690713751));
#33981=CARTESIAN_POINT('',(54.9397894030341,35.9543320991532,33.3227466489021));
#33982=CARTESIAN_POINT('',(56.9397894030342,37.9543320991532,33.3227466489021));
#33983=CARTESIAN_POINT('Origin',(54.9397894030341,37.9543320991532,33.3227466489021));
#33984=CARTESIAN_POINT('Origin',(54.9397894030341,37.9543320991532,33.3227466489021));
#33985=CARTESIAN_POINT('',(56.9397894030341,37.9543320991532,8.12867690713751));
#33986=CARTESIAN_POINT('Origin',(54.9397894030341,37.9543320991532,33.0496657090004));
#33987=CARTESIAN_POINT('',(56.9397894030342,37.9543320991532,32.7765847690986));
#33988=CARTESIAN_POINT('',(54.9397894030341,39.9543320991532,32.7765847690986));
#33989=CARTESIAN_POINT('Origin',(54.9397894030341,37.9543320991532,32.7765847690986));
#33990=CARTESIAN_POINT('Origin',(54.9397894030341,37.9543320991532,32.7765847690986));
#33991=CARTESIAN_POINT('',(54.9397894030341,39.5643320991532,33.0496657090004));
#33992=CARTESIAN_POINT('',(54.9397894030341,39.5643320991532,33.0496657090004));
#33993=CARTESIAN_POINT('',(54.9397894030341,36.3443320991532,33.0496657090004));
#33994=CARTESIAN_POINT('Origin',(54.9397894030341,37.9543320991532,33.0496657090004));
#33995=CARTESIAN_POINT('Origin',(54.9397894030341,37.9543320991532,33.0496657090004));
#33996=CARTESIAN_POINT('Origin',(54.9397894030341,37.9543320991532,33.3227466489021));
#33997=CARTESIAN_POINT('',(54.9397894030341,35.9543320991532,33.3227466489021));
#33998=CARTESIAN_POINT('Origin',(54.9397894030341,37.9543320991532,8.12867690713751));
#33999=CARTESIAN_POINT('',(54.9397894030341,35.9543320991532,32.6628133155688));
#34000=CARTESIAN_POINT('',(56.9397894030342,37.9543320991532,32.6628133155688));
#34001=CARTESIAN_POINT('Origin',(54.9397894030341,37.9543320991532,32.6628133155688));
#34002=CARTESIAN_POINT('Origin',(54.9397894030341,37.9543320991532,32.6628133155688));
#34003=CARTESIAN_POINT('',(56.9397894030341,37.9543320991532,8.12867690713751));
#34004=CARTESIAN_POINT('Origin',(54.9397894030341,37.9543320991532,32.389732375667));
#34005=CARTESIAN_POINT('',(56.9397894030342,37.9543320991532,32.1166514357652));
#34006=CARTESIAN_POINT('',(54.9397894030341,39.9543320991532,32.1166514357652));
#34007=CARTESIAN_POINT('Origin',(54.9397894030341,37.9543320991532,32.1166514357652));
#34008=CARTESIAN_POINT('Origin',(54.9397894030341,37.9543320991532,32.1166514357652));
#34009=CARTESIAN_POINT('',(54.9397894030341,39.5643320991532,32.389732375667));
#34010=CARTESIAN_POINT('',(54.9397894030341,39.5643320991532,32.389732375667));
#34011=CARTESIAN_POINT('',(54.9397894030341,36.3443320991532,32.389732375667));
#34012=CARTESIAN_POINT('Origin',(54.9397894030341,37.9543320991532,32.389732375667));
#34013=CARTESIAN_POINT('Origin',(54.9397894030341,37.9543320991532,32.389732375667));
#34014=CARTESIAN_POINT('Origin',(54.9397894030341,37.9543320991532,32.6628133155688));
#34015=CARTESIAN_POINT('',(54.9397894030341,35.9543320991532,32.6628133155688));
#34016=CARTESIAN_POINT('Origin',(54.9397894030341,37.9543320991532,8.12867690713751));
#34017=CARTESIAN_POINT('',(54.9397894030341,35.9543320991532,32.0028799822355));
#34018=CARTESIAN_POINT('',(56.9397894030342,37.9543320991532,32.0028799822355));
#34019=CARTESIAN_POINT('Origin',(54.9397894030341,37.9543320991532,32.0028799822355));
#34020=CARTESIAN_POINT('Origin',(54.9397894030341,37.9543320991532,32.0028799822355));
#34021=CARTESIAN_POINT('',(56.9397894030341,37.9543320991532,8.12867690713751));
#34022=CARTESIAN_POINT('Origin',(54.9397894030341,37.9543320991532,31.7297990423337));
#34023=CARTESIAN_POINT('',(56.9397894030342,37.9543320991532,31.4567181024319));
#34024=CARTESIAN_POINT('',(54.9397894030341,39.9543320991532,31.4567181024319));
#34025=CARTESIAN_POINT('Origin',(54.9397894030341,37.9543320991532,31.4567181024319));
#34026=CARTESIAN_POINT('Origin',(54.9397894030341,37.9543320991532,31.4567181024319));
#34027=CARTESIAN_POINT('',(54.9397894030341,39.5643320991532,31.7297990423337));
#34028=CARTESIAN_POINT('',(54.9397894030341,39.5643320991532,31.7297990423337));
#34029=CARTESIAN_POINT('',(54.9397894030341,36.3443320991532,31.7297990423337));
#34030=CARTESIAN_POINT('Origin',(54.9397894030341,37.9543320991532,31.7297990423337));
#34031=CARTESIAN_POINT('Origin',(54.9397894030341,37.9543320991532,31.7297990423337));
#34032=CARTESIAN_POINT('Origin',(54.9397894030341,37.9543320991532,32.0028799822355));
#34033=CARTESIAN_POINT('',(54.9397894030341,35.9543320991532,32.0028799822355));
#34034=CARTESIAN_POINT('Origin',(54.9397894030341,37.9543320991532,8.12867690713751));
#34035=CARTESIAN_POINT('',(54.9397894030341,35.9543320991532,31.3429466489021));
#34036=CARTESIAN_POINT('',(56.9397894030342,37.9543320991532,31.3429466489021));
#34037=CARTESIAN_POINT('Origin',(54.9397894030341,37.9543320991532,31.3429466489021));
#34038=CARTESIAN_POINT('Origin',(54.9397894030341,37.9543320991532,31.3429466489021));
#34039=CARTESIAN_POINT('',(56.9397894030341,37.9543320991532,8.12867690713751));
#34040=CARTESIAN_POINT('Origin',(54.9397894030341,37.9543320991532,31.0698657090004));
#34041=CARTESIAN_POINT('',(56.9397894030342,37.9543320991532,30.7967847690986));
#34042=CARTESIAN_POINT('',(54.9397894030341,39.9543320991532,30.7967847690986));
#34043=CARTESIAN_POINT('Origin',(54.9397894030341,37.9543320991532,30.7967847690986));
#34044=CARTESIAN_POINT('Origin',(54.9397894030341,37.9543320991532,30.7967847690986));
#34045=CARTESIAN_POINT('',(54.9397894030341,39.5643320991532,31.0698657090004));
#34046=CARTESIAN_POINT('',(54.9397894030341,39.5643320991532,31.0698657090004));
#34047=CARTESIAN_POINT('',(54.9397894030341,36.3443320991532,31.0698657090004));
#34048=CARTESIAN_POINT('Origin',(54.9397894030341,37.9543320991532,31.0698657090004));
#34049=CARTESIAN_POINT('Origin',(54.9397894030341,37.9543320991532,31.0698657090004));
#34050=CARTESIAN_POINT('Origin',(54.9397894030341,37.9543320991532,31.3429466489021));
#34051=CARTESIAN_POINT('',(54.9397894030341,35.9543320991532,31.3429466489021));
#34052=CARTESIAN_POINT('Origin',(54.9397894030341,37.9543320991532,8.12867690713751));
#34053=CARTESIAN_POINT('',(54.9397894030341,35.9543320991532,30.6830133155688));
#34054=CARTESIAN_POINT('',(56.9397894030342,37.9543320991532,30.6830133155688));
#34055=CARTESIAN_POINT('Origin',(54.9397894030341,37.9543320991532,30.6830133155688));
#34056=CARTESIAN_POINT('Origin',(54.9397894030341,37.9543320991532,30.6830133155688));
#34057=CARTESIAN_POINT('',(56.9397894030341,37.9543320991532,8.12867690713751));
#34058=CARTESIAN_POINT('Origin',(54.9397894030341,37.9543320991532,30.409932375667));
#34059=CARTESIAN_POINT('',(56.9397894030342,37.9543320991532,30.1368514357652));
#34060=CARTESIAN_POINT('',(54.9397894030341,39.9543320991532,30.1368514357652));
#34061=CARTESIAN_POINT('Origin',(54.9397894030341,37.9543320991532,30.1368514357652));
#34062=CARTESIAN_POINT('Origin',(54.9397894030341,37.9543320991532,30.1368514357652));
#34063=CARTESIAN_POINT('',(54.9397894030341,39.5643320991532,30.409932375667));
#34064=CARTESIAN_POINT('',(54.9397894030341,39.5643320991532,30.409932375667));
#34065=CARTESIAN_POINT('',(54.9397894030341,36.3443320991532,30.409932375667));
#34066=CARTESIAN_POINT('Origin',(54.9397894030341,37.9543320991532,30.409932375667));
#34067=CARTESIAN_POINT('Origin',(54.9397894030341,37.9543320991532,30.409932375667));
#34068=CARTESIAN_POINT('Origin',(54.9397894030341,37.9543320991532,30.6830133155688));
#34069=CARTESIAN_POINT('',(54.9397894030341,35.9543320991532,30.6830133155688));
#34070=CARTESIAN_POINT('Origin',(54.9397894030341,37.9543320991532,8.12867690713751));
#34071=CARTESIAN_POINT('',(54.9397894030341,35.9543320991532,30.0230799822355));
#34072=CARTESIAN_POINT('',(56.9397894030342,37.9543320991532,30.0230799822355));
#34073=CARTESIAN_POINT('Origin',(54.9397894030341,37.9543320991532,30.0230799822355));
#34074=CARTESIAN_POINT('Origin',(54.9397894030341,37.9543320991532,30.0230799822355));
#34075=CARTESIAN_POINT('',(56.9397894030341,37.9543320991532,8.12867690713751));
#34076=CARTESIAN_POINT('Origin',(54.9397894030341,37.9543320991532,29.7499990423337));
#34077=CARTESIAN_POINT('',(56.9397894030342,37.9543320991532,29.4769181024319));
#34078=CARTESIAN_POINT('',(54.9397894030341,39.9543320991532,29.4769181024319));
#34079=CARTESIAN_POINT('Origin',(54.9397894030341,37.9543320991532,29.4769181024319));
#34080=CARTESIAN_POINT('Origin',(54.9397894030341,37.9543320991532,29.4769181024319));
#34081=CARTESIAN_POINT('',(54.9397894030341,39.5643320991532,29.7499990423337));
#34082=CARTESIAN_POINT('',(54.9397894030341,39.5643320991532,29.7499990423337));
#34083=CARTESIAN_POINT('',(54.9397894030341,36.3443320991532,29.7499990423337));
#34084=CARTESIAN_POINT('Origin',(54.9397894030341,37.9543320991532,29.7499990423337));
#34085=CARTESIAN_POINT('Origin',(54.9397894030341,37.9543320991532,29.7499990423337));
#34086=CARTESIAN_POINT('Origin',(54.9397894030341,37.9543320991532,30.0230799822355));
#34087=CARTESIAN_POINT('',(54.9397894030341,35.9543320991532,30.0230799822355));
#34088=CARTESIAN_POINT('Origin',(54.9397894030341,37.9543320991532,8.12867690713751));
#34089=CARTESIAN_POINT('',(54.9397894030341,35.9543320991532,29.3631466489021));
#34090=CARTESIAN_POINT('',(56.9397894030342,37.9543320991532,29.3631466489021));
#34091=CARTESIAN_POINT('Origin',(54.9397894030341,37.9543320991532,29.3631466489021));
#34092=CARTESIAN_POINT('Origin',(54.9397894030341,37.9543320991532,29.3631466489021));
#34093=CARTESIAN_POINT('',(56.9397894030341,37.9543320991532,8.12867690713751));
#34094=CARTESIAN_POINT('Origin',(54.9397894030341,37.9543320991532,29.0900657090004));
#34095=CARTESIAN_POINT('',(56.9397894030342,37.9543320991532,28.8169847690986));
#34096=CARTESIAN_POINT('',(54.9397894030341,39.9543320991532,28.8169847690986));
#34097=CARTESIAN_POINT('Origin',(54.9397894030341,37.9543320991532,28.8169847690986));
#34098=CARTESIAN_POINT('Origin',(54.9397894030341,37.9543320991532,28.8169847690986));
#34099=CARTESIAN_POINT('',(54.9397894030341,39.5643320991532,29.0900657090004));
#34100=CARTESIAN_POINT('',(54.9397894030341,39.5643320991532,29.0900657090004));
#34101=CARTESIAN_POINT('',(54.9397894030341,36.3443320991532,29.0900657090004));
#34102=CARTESIAN_POINT('Origin',(54.9397894030341,37.9543320991532,29.0900657090004));
#34103=CARTESIAN_POINT('Origin',(54.9397894030341,37.9543320991532,29.0900657090004));
#34104=CARTESIAN_POINT('Origin',(54.9397894030341,37.9543320991532,29.3631466489021));
#34105=CARTESIAN_POINT('',(54.9397894030341,35.9543320991532,29.3631466489021));
#34106=CARTESIAN_POINT('Origin',(54.9397894030341,37.9543320991532,8.12867690713751));
#34107=CARTESIAN_POINT('',(54.9397894030341,35.9543320991532,28.7032133155688));
#34108=CARTESIAN_POINT('',(56.9397894030342,37.9543320991532,28.7032133155688));
#34109=CARTESIAN_POINT('Origin',(54.9397894030341,37.9543320991532,28.7032133155688));
#34110=CARTESIAN_POINT('Origin',(54.9397894030341,37.9543320991532,28.7032133155688));
#34111=CARTESIAN_POINT('',(56.9397894030341,37.9543320991532,8.12867690713751));
#34112=CARTESIAN_POINT('Origin',(54.9397894030341,37.9543320991532,28.430132375667));
#34113=CARTESIAN_POINT('',(56.9397894030342,37.9543320991532,28.1570514357652));
#34114=CARTESIAN_POINT('',(54.9397894030341,39.9543320991532,28.1570514357652));
#34115=CARTESIAN_POINT('Origin',(54.9397894030341,37.9543320991532,28.1570514357652));
#34116=CARTESIAN_POINT('Origin',(54.9397894030341,37.9543320991532,28.1570514357652));
#34117=CARTESIAN_POINT('',(54.9397894030341,39.5643320991532,28.430132375667));
#34118=CARTESIAN_POINT('',(54.9397894030341,39.5643320991532,28.430132375667));
#34119=CARTESIAN_POINT('',(54.9397894030341,36.3443320991532,28.430132375667));
#34120=CARTESIAN_POINT('Origin',(54.9397894030341,37.9543320991532,28.430132375667));
#34121=CARTESIAN_POINT('Origin',(54.9397894030341,37.9543320991532,28.430132375667));
#34122=CARTESIAN_POINT('Origin',(54.9397894030341,37.9543320991532,28.7032133155688));
#34123=CARTESIAN_POINT('',(54.9397894030341,35.9543320991532,28.7032133155688));
#34124=CARTESIAN_POINT('Origin',(54.9397894030341,37.9543320991532,8.12867690713751));
#34125=CARTESIAN_POINT('',(54.9397894030341,35.9543320991532,28.0432799822355));
#34126=CARTESIAN_POINT('',(56.9397894030342,37.9543320991532,28.0432799822355));
#34127=CARTESIAN_POINT('Origin',(54.9397894030341,37.9543320991532,28.0432799822355));
#34128=CARTESIAN_POINT('Origin',(54.9397894030341,37.9543320991532,28.0432799822355));
#34129=CARTESIAN_POINT('',(56.9397894030341,37.9543320991532,8.12867690713751));
#34130=CARTESIAN_POINT('Origin',(54.9397894030341,37.9543320991532,27.7701990423337));
#34131=CARTESIAN_POINT('',(56.9397894030342,37.9543320991532,27.4971181024319));
#34132=CARTESIAN_POINT('',(54.9397894030341,39.9543320991532,27.4971181024319));
#34133=CARTESIAN_POINT('Origin',(54.9397894030341,37.9543320991532,27.4971181024319));
#34134=CARTESIAN_POINT('Origin',(54.9397894030341,37.9543320991532,27.4971181024319));
#34135=CARTESIAN_POINT('',(54.9397894030341,39.5643320991532,27.7701990423337));
#34136=CARTESIAN_POINT('',(54.9397894030341,39.5643320991532,27.7701990423337));
#34137=CARTESIAN_POINT('',(54.9397894030341,36.3443320991532,27.7701990423337));
#34138=CARTESIAN_POINT('Origin',(54.9397894030341,37.9543320991532,27.7701990423337));
#34139=CARTESIAN_POINT('Origin',(54.9397894030341,37.9543320991532,27.7701990423337));
#34140=CARTESIAN_POINT('Origin',(54.9397894030341,37.9543320991532,28.0432799822355));
#34141=CARTESIAN_POINT('',(54.9397894030341,35.9543320991532,28.0432799822355));
#34142=CARTESIAN_POINT('Origin',(54.9397894030341,37.9543320991532,8.12867690713751));
#34143=CARTESIAN_POINT('',(54.9397894030341,35.9543320991532,27.3833466489021));
#34144=CARTESIAN_POINT('',(56.9397894030342,37.9543320991532,27.3833466489021));
#34145=CARTESIAN_POINT('Origin',(54.9397894030341,37.9543320991532,27.3833466489021));
#34146=CARTESIAN_POINT('Origin',(54.9397894030341,37.9543320991532,27.3833466489021));
#34147=CARTESIAN_POINT('',(56.9397894030341,37.9543320991532,8.12867690713751));
#34148=CARTESIAN_POINT('Origin',(54.9397894030341,37.9543320991532,27.1102657090004));
#34149=CARTESIAN_POINT('',(56.9397894030342,37.9543320991532,26.8371847690986));
#34150=CARTESIAN_POINT('',(54.9397894030341,39.9543320991532,26.8371847690986));
#34151=CARTESIAN_POINT('Origin',(54.9397894030341,37.9543320991532,26.8371847690986));
#34152=CARTESIAN_POINT('Origin',(54.9397894030341,37.9543320991532,26.8371847690986));
#34153=CARTESIAN_POINT('',(54.9397894030341,39.5643320991532,27.1102657090004));
#34154=CARTESIAN_POINT('',(54.9397894030341,39.5643320991532,27.1102657090004));
#34155=CARTESIAN_POINT('',(54.9397894030341,36.3443320991532,27.1102657090004));
#34156=CARTESIAN_POINT('Origin',(54.9397894030341,37.9543320991532,27.1102657090004));
#34157=CARTESIAN_POINT('Origin',(54.9397894030341,37.9543320991532,27.1102657090004));
#34158=CARTESIAN_POINT('Origin',(54.9397894030341,37.9543320991532,27.3833466489021));
#34159=CARTESIAN_POINT('',(54.9397894030341,35.9543320991532,27.3833466489021));
#34160=CARTESIAN_POINT('Origin',(54.9397894030341,37.9543320991532,8.12867690713751));
#34161=CARTESIAN_POINT('',(54.9397894030341,35.9543320991532,26.7234133155688));
#34162=CARTESIAN_POINT('',(56.9397894030342,37.9543320991532,26.7234133155688));
#34163=CARTESIAN_POINT('Origin',(54.9397894030341,37.9543320991532,26.7234133155688));
#34164=CARTESIAN_POINT('Origin',(54.9397894030341,37.9543320991532,26.7234133155688));
#34165=CARTESIAN_POINT('',(56.9397894030341,37.9543320991532,8.12867690713751));
#34166=CARTESIAN_POINT('Origin',(54.9397894030341,37.9543320991532,26.450332375667));
#34167=CARTESIAN_POINT('',(56.9397894030341,37.9543320991532,26.1772514357652));
#34168=CARTESIAN_POINT('',(54.9397894030341,39.9543320991532,26.1772514357652));
#34169=CARTESIAN_POINT('Origin',(54.9397894030341,37.9543320991532,26.1772514357652));
#34170=CARTESIAN_POINT('Origin',(54.9397894030341,37.9543320991532,26.1772514357652));
#34171=CARTESIAN_POINT('',(54.9397894030341,39.5643320991532,26.450332375667));
#34172=CARTESIAN_POINT('',(54.9397894030341,39.5643320991532,26.450332375667));
#34173=CARTESIAN_POINT('',(54.9397894030341,36.3443320991532,26.450332375667));
#34174=CARTESIAN_POINT('Origin',(54.9397894030341,37.9543320991532,26.450332375667));
#34175=CARTESIAN_POINT('Origin',(54.9397894030341,37.9543320991532,26.450332375667));
#34176=CARTESIAN_POINT('Origin',(54.9397894030341,37.9543320991532,26.7234133155688));
#34177=CARTESIAN_POINT('',(54.9397894030341,35.9543320991532,26.7234133155688));
#34178=CARTESIAN_POINT('Origin',(54.9397894030341,37.9543320991532,8.12867690713751));
#34179=CARTESIAN_POINT('',(54.9397894030341,35.9543320991532,26.0634799822355));
#34180=CARTESIAN_POINT('',(56.9397894030341,37.9543320991532,26.0634799822355));
#34181=CARTESIAN_POINT('Origin',(54.9397894030341,37.9543320991532,26.0634799822355));
#34182=CARTESIAN_POINT('Origin',(54.9397894030341,37.9543320991532,26.0634799822355));
#34183=CARTESIAN_POINT('',(56.9397894030341,37.9543320991532,8.12867690713751));
#34184=CARTESIAN_POINT('Origin',(54.9397894030341,37.9543320991532,25.7903990423337));
#34185=CARTESIAN_POINT('',(56.9397894030341,37.9543320991532,25.5173181024319));
#34186=CARTESIAN_POINT('',(54.9397894030341,39.9543320991532,25.5173181024319));
#34187=CARTESIAN_POINT('Origin',(54.9397894030341,37.9543320991532,25.5173181024319));
#34188=CARTESIAN_POINT('Origin',(54.9397894030341,37.9543320991532,25.5173181024319));
#34189=CARTESIAN_POINT('',(54.9397894030341,39.5643320991532,25.7903990423337));
#34190=CARTESIAN_POINT('',(54.9397894030341,39.5643320991532,25.7903990423337));
#34191=CARTESIAN_POINT('',(54.9397894030341,36.3443320991532,25.7903990423337));
#34192=CARTESIAN_POINT('Origin',(54.9397894030341,37.9543320991532,25.7903990423337));
#34193=CARTESIAN_POINT('Origin',(54.9397894030341,37.9543320991532,25.7903990423337));
#34194=CARTESIAN_POINT('Origin',(54.9397894030341,37.9543320991532,26.0634799822355));
#34195=CARTESIAN_POINT('',(54.9397894030341,35.9543320991532,26.0634799822355));
#34196=CARTESIAN_POINT('Origin',(54.9397894030341,37.9543320991532,8.12867690713751));
#34197=CARTESIAN_POINT('',(54.9397894030341,35.9543320991532,25.4035466489021));
#34198=CARTESIAN_POINT('',(56.9397894030341,37.9543320991532,25.4035466489021));
#34199=CARTESIAN_POINT('Origin',(54.9397894030341,37.9543320991532,25.4035466489021));
#34200=CARTESIAN_POINT('Origin',(54.9397894030341,37.9543320991532,25.4035466489021));
#34201=CARTESIAN_POINT('',(56.9397894030341,37.9543320991532,8.12867690713751));
#34202=CARTESIAN_POINT('Origin',(54.9397894030341,37.9543320991532,25.1304657090004));
#34203=CARTESIAN_POINT('',(56.9397894030341,37.9543320991532,24.8573847690986));
#34204=CARTESIAN_POINT('',(54.9397894030341,39.9543320991532,24.8573847690986));
#34205=CARTESIAN_POINT('Origin',(54.9397894030341,37.9543320991532,24.8573847690986));
#34206=CARTESIAN_POINT('Origin',(54.9397894030341,37.9543320991532,24.8573847690986));
#34207=CARTESIAN_POINT('',(54.9397894030341,39.5643320991532,25.1304657090004));
#34208=CARTESIAN_POINT('',(54.9397894030341,39.5643320991532,25.1304657090004));
#34209=CARTESIAN_POINT('',(54.9397894030341,36.3443320991532,25.1304657090004));
#34210=CARTESIAN_POINT('Origin',(54.9397894030341,37.9543320991532,25.1304657090004));
#34211=CARTESIAN_POINT('Origin',(54.9397894030341,37.9543320991532,25.1304657090004));
#34212=CARTESIAN_POINT('Origin',(54.9397894030341,37.9543320991532,25.4035466489021));
#34213=CARTESIAN_POINT('',(54.9397894030341,35.9543320991532,25.4035466489021));
#34214=CARTESIAN_POINT('Origin',(54.9397894030341,37.9543320991532,19.9294657090004));
#34215=CARTESIAN_POINT('',(63.1147876185643,37.9489306105332,19.9294657090004));
#34216=CARTESIAN_POINT('',(62.8131508375241,38.1149705811106,19.6294657090004));
#34217=CARTESIAN_POINT('Ctrl Pts',(63.1147876185643,37.9489306105332,19.9294657090003));
#34218=CARTESIAN_POINT('Ctrl Pts',(62.9611501927074,38.0335023712479,19.7757724373647));
#34219=CARTESIAN_POINT('Ctrl Pts',(62.8131508375241,38.1149705811106,19.6294657090003));
#34220=CARTESIAN_POINT('',(63.1082046987747,37.6262824743835,19.9294657090004));
#34221=CARTESIAN_POINT('Origin',(54.9397894030341,37.9543320991532,19.9294657090004));
#34222=CARTESIAN_POINT('',(62.8000464044319,37.4726840201813,19.6294657090004));
#34223=CARTESIAN_POINT('Ctrl Pts',(62.8000464044319,37.4726840201813,19.6294657090003));
#34224=CARTESIAN_POINT('Ctrl Pts',(62.951245567544,37.5480477477104,19.7757724373647));
#34225=CARTESIAN_POINT('Ctrl Pts',(63.1082046987747,37.6262824743835,19.9294657090003));
#34226=CARTESIAN_POINT('',(63.0871457149245,37.2826103359947,19.9294657090004));
#34227=CARTESIAN_POINT('Ctrl Pts',(63.0871457149245,37.2826103359947,19.9294657090003));
#34228=CARTESIAN_POINT('Ctrl Pts',(62.9409128885521,37.3794235676598,19.7757724373647));
#34229=CARTESIAN_POINT('Ctrl Pts',(62.8000464044319,37.4726840201813,19.6294657090004));
#34230=CARTESIAN_POINT('',(63.0542858808421,36.9615723539771,19.9294657090004));
#34231=CARTESIAN_POINT('Origin',(54.9397894030341,37.9543320991532,19.9294657090004));
#34232=CARTESIAN_POINT('',(62.7346332578465,36.8336027477512,19.6294657090004));
#34233=CARTESIAN_POINT('Ctrl Pts',(62.7346332578465,36.8336027477512,19.6294657090003));
#34234=CARTESIAN_POINT('Ctrl Pts',(62.8914721616528,36.8963915732358,19.7757724373647));
#34235=CARTESIAN_POINT('Ctrl Pts',(63.0542858808421,36.9615723539771,19.9294657090003));
#34236=CARTESIAN_POINT('',(63.0052844992482,36.6207602589636,19.9294657090004));
#34237=CARTESIAN_POINT('Ctrl Pts',(63.0052844992482,36.6207602589636,19.9294657090003));
#34238=CARTESIAN_POINT('Ctrl Pts',(62.8674294276931,36.7291706854956,19.7757724373646));
#34239=CARTESIAN_POINT('Ctrl Pts',(62.7346332578465,36.8336027477512,19.6294657090003));
#34240=CARTESIAN_POINT('',(62.9463664276474,36.3034688858809,19.9294657090004));
#34241=CARTESIAN_POINT('Origin',(54.9397894030341,37.9543320991532,19.9294657090004));
#34242=CARTESIAN_POINT('',(62.617346711466,36.2019797442473,19.6294657090004));
#34243=CARTESIAN_POINT('Ctrl Pts',(62.617346711466,36.2019797442473,19.6294657090004));
#34244=CARTESIAN_POINT('Ctrl Pts',(62.7787816189382,36.2517758184133,19.7757724373647));
#34245=CARTESIAN_POINT('Ctrl Pts',(62.9463664276474,36.3034688858809,19.9294657090003));
#34246=CARTESIAN_POINT('',(62.8697487444197,35.9677848825051,19.9294657090004));
#34247=CARTESIAN_POINT('Ctrl Pts',(62.8697487444197,35.9677848825052,19.9294657090003));
#34248=CARTESIAN_POINT('Ctrl Pts',(62.7411888304386,36.0870710504019,19.7757724373647));
#34249=CARTESIAN_POINT('Ctrl Pts',(62.617346711466,36.2019797442473,19.6294657090004));
#34250=CARTESIAN_POINT('',(62.785164525346,35.6563516400959,19.9294657090004));
#34251=CARTESIAN_POINT('Origin',(54.9397894030341,37.9543320991532,19.9294657090004));
#34252=CARTESIAN_POINT('',(62.4489672879057,35.5820183565476,19.6294657090004));
#34253=CARTESIAN_POINT('Ctrl Pts',(62.4489672879057,35.5820183565476,19.6294657090004));
#34254=CARTESIAN_POINT('Ctrl Pts',(62.6139238763694,35.6184902947372,19.7757724373647));
#34255=CARTESIAN_POINT('Ctrl Pts',(62.785164525346,35.6563516400959,19.9294657090003));
#34256=CARTESIAN_POINT('',(62.6814404185254,35.3280296500162,19.9294657090004));
#34257=CARTESIAN_POINT('Ctrl Pts',(62.6814404185254,35.3280296500162,19.9294657090003));
#34258=CARTESIAN_POINT('Ctrl Pts',(62.563031207135,35.4573977295112,19.7757724373647));
#34259=CARTESIAN_POINT('Ctrl Pts',(62.4489672879057,35.5820183565476,19.6294657090004));
#34260=CARTESIAN_POINT('',(62.5717529460015,35.0245270751257,19.9294657090004));
#34261=CARTESIAN_POINT('Origin',(54.9397894030341,37.9543320991532,19.9294657090004));
#34262=CARTESIAN_POINT('',(62.2306155244487,34.9778443254007,19.6294657090004));
#34263=CARTESIAN_POINT('Ctrl Pts',(62.2306155244487,34.9778443254006,19.6294657090004));
#34264=CARTESIAN_POINT('Ctrl Pts',(62.3979960350237,35.0007494128826,19.7757724373647));
#34265=CARTESIAN_POINT('Ctrl Pts',(62.5717529460015,35.0245270751257,19.9294657090004));
#34266=CARTESIAN_POINT('',(62.4416126824056,34.705752027017,19.9294657090004));
#34267=CARTESIAN_POINT('Ctrl Pts',(62.4416126824056,34.705752027017,19.9294657090003));
#34268=CARTESIAN_POINT('Ctrl Pts',(62.3341421673715,34.8443410948853,19.7757724373647));
#34269=CARTESIAN_POINT('Ctrl Pts',(62.2306155244488,34.9778443254007,19.6294657090004));
#34270=CARTESIAN_POINT('',(62.3075519084639,34.4121998792067,19.9294657090004));
#34271=CARTESIAN_POINT('Origin',(54.9397894030341,37.9543320991532,19.9294657090004));
#34272=CARTESIAN_POINT('',(61.9637445160554,34.3934783293021,19.6294657090004));
#34273=CARTESIAN_POINT('Ctrl Pts',(61.9637445160554,34.3934783293021,19.6294657090004));
#34274=CARTESIAN_POINT('Ctrl Pts',(62.1324350590596,34.4026641364983,19.7757724373647));
#34275=CARTESIAN_POINT('Ctrl Pts',(62.3075519084639,34.4121998792067,19.9294657090004));
#34276=CARTESIAN_POINT('',(62.1518615500752,34.1050931684198,19.9294657090004));
#34277=CARTESIAN_POINT('Ctrl Pts',(62.1518615500752,34.1050931684198,19.9294657090003));
#34278=CARTESIAN_POINT('Ctrl Pts',(62.0560449299436,34.2519809372804,19.7757724373647));
#34279=CARTESIAN_POINT('Ctrl Pts',(61.9637445160554,34.3934783293021,19.6294657090004));
#34280=CARTESIAN_POINT('',(61.9943196270479,33.8234449888007,19.9294657090004));
#34281=CARTESIAN_POINT('Origin',(54.9397894030341,37.9543320991532,19.9294657090004));
#34282=CARTESIAN_POINT('',(61.6501302452559,33.8328092275425,19.6294657090004));
#34283=CARTESIAN_POINT('Ctrl Pts',(61.6501302452559,33.8328092275425,19.6294657090003));
#34284=CARTESIAN_POINT('Ctrl Pts',(61.8190082129576,33.8282146244215,19.7757724373647));
#34285=CARTESIAN_POINT('Ctrl Pts',(61.9943196270479,33.8234449888008,19.9294657090004));
#34286=CARTESIAN_POINT('',(61.8141152675145,33.5300503598269,19.9294657090004));
#34287=CARTESIAN_POINT('Ctrl Pts',(61.8141152675145,33.5300503598269,19.9294657090003));
#34288=CARTESIAN_POINT('Ctrl Pts',(61.7305901860837,33.6842593158128,19.7757724373647));
#34289=CARTESIAN_POINT('Ctrl Pts',(61.6501302452559,33.8328092275425,19.6294657090003));
#34290=CARTESIAN_POINT('',(61.6341406109067,33.2621804705658,19.9294657090004));
#34291=CARTESIAN_POINT('Origin',(54.9397894030341,37.9543320991532,19.9294657090004));
#34292=CARTESIAN_POINT('',(61.2918597632797,33.2995681804899,19.6294657090004));
#34293=CARTESIAN_POINT('Ctrl Pts',(61.2918597632797,33.2995681804899,19.6294657090003));
#34294=CARTESIAN_POINT('Ctrl Pts',(61.4598013006668,33.2812237433776,19.7757724373647));
#34295=CARTESIAN_POINT('Ctrl Pts',(61.6341406109066,33.2621804705658,19.9294657090003));
#34296=CARTESIAN_POINT('',(61.4306214805095,32.9844504162541,19.9294657090004));
#34297=CARTESIAN_POINT('Ctrl Pts',(61.4306214805096,32.9844504162541,19.9294657090003));
#34298=CARTESIAN_POINT('Ctrl Pts',(61.3599437834159,33.144954324206,19.7757724373647));
#34299=CARTESIAN_POINT('Ctrl Pts',(61.2918597632797,33.2995681804899,19.6294657090004));
#34300=CARTESIAN_POINT('',(61.2294117919672,32.7321414472685,19.9294657090004));
#34301=CARTESIAN_POINT('Origin',(54.9397894030341,37.9543320991532,19.9294657090004));
#34302=CARTESIAN_POINT('',(60.891317301074,32.7973038193341,19.6294657090004));
#34303=CARTESIAN_POINT('Ctrl Pts',(60.891317301074,32.7973038193341,19.6294657090003));
#34304=CARTESIAN_POINT('Ctrl Pts',(61.0572047849235,32.7653316274328,19.7757724373647));
#34305=CARTESIAN_POINT('Ctrl Pts',(61.2294117919672,32.7321414472685,19.9294657090003));
#34306=CARTESIAN_POINT('',(61.0039322769409,32.4719242153082,19.9294657090004));
#34307=CARTESIAN_POINT('Ctrl Pts',(61.0039322769409,32.4719242153082,19.9294657090003));
#34308=CARTESIAN_POINT('Ctrl Pts',(60.9465723125975,32.6376549481999,19.7757724373647));
#34309=CARTESIAN_POINT('Ctrl Pts',(60.891317301074,32.7973038193342,19.6294657090004));
#34310=CARTESIAN_POINT('',(60.7828265737441,32.2368552411588,19.9294657090004));
#34311=CARTESIAN_POINT('Origin',(54.9397894030341,37.9543320991532,19.9294657090004));
#34312=CARTESIAN_POINT('',(60.4511684026397,32.3293586305308,19.6294657090004));
#34313=CARTESIAN_POINT('Ctrl Pts',(60.4511684026397,32.3293586305308,19.6294657090003));
#34314=CARTESIAN_POINT('Ctrl Pts',(60.6138978791162,32.2839714535025,19.7757724373647));
#34315=CARTESIAN_POINT('Ctrl Pts',(60.7828265737441,32.2368552411588,19.9294657090003));
#34316=CARTESIAN_POINT('',(60.5368872030596,31.9958825342957,19.9294657090004));
#34317=CARTESIAN_POINT('Ctrl Pts',(60.5368872030596,31.9958825342957,19.9294657090003));
#34318=CARTESIAN_POINT('Ctrl Pts',(60.4932266925654,32.1657371814435,19.7757724373647));
#34319=CARTESIAN_POINT('Ctrl Pts',(60.4511684026397,32.3293586305308,19.6294657090003));
#34320=CARTESIAN_POINT('',(60.2973569071831,31.7796179002217,19.9294657090004));
#34321=CARTESIAN_POINT('Origin',(54.9397894030341,37.9543320991532,19.9294657090004));
#34322=CARTESIAN_POINT('',(59.9743421862767,31.8988467121058,19.6294657090004));
#34323=CARTESIAN_POINT('Ctrl Pts',(59.9743421862767,31.8988467121058,19.6294657090003));
#34324=CARTESIAN_POINT('Ctrl Pts',(60.1328307175625,31.8403465941253,19.7757724373647));
#34325=CARTESIAN_POINT('Ctrl Pts',(60.2973569071831,31.7796179002217,19.9294657090003));
#34326=CARTESIAN_POINT('',(60.0325943667752,31.5594933520624,19.9294657090004));
#34327=CARTESIAN_POINT('Ctrl Pts',(60.0325943667752,31.5594933520624,19.9294657090003));
#34328=CARTESIAN_POINT('Ctrl Pts',(60.0029238636241,31.7323415588135,19.7757724373647));
#34329=CARTESIAN_POINT('Ctrl Pts',(59.9743421862767,31.8988467121058,19.6294657090003));
#34330=CARTESIAN_POINT('',(59.7762335128185,31.3634722635224,19.9294657090004));
#34331=CARTESIAN_POINT('Origin',(54.9397894030341,37.9543320991532,19.9294657090004));
#34332=CARTESIAN_POINT('',(59.4640118517838,31.5086330498468,19.6294657090004));
#34333=CARTESIAN_POINT('Ctrl Pts',(59.4640118517838,31.5086330498468,19.6294657090004));
#34334=CARTESIAN_POINT('Ctrl Pts',(59.6172047228522,31.4374092995474,19.7757724373647));
#34335=CARTESIAN_POINT('Ctrl Pts',(59.7762335128185,31.3634722635223,19.9294657090003));
#34336=CARTESIAN_POINT('',(59.4944097537108,31.1656607666168,19.9294657090004));
#34337=CARTESIAN_POINT('Ctrl Pts',(59.4944097537108,31.1656607666168,19.9294657090003));
#34338=CARTESIAN_POINT('Ctrl Pts',(59.478926710206,31.3403522566732,19.7757724373647));
#34339=CARTESIAN_POINT('Ctrl Pts',(59.4640118517839,31.5086330498468,19.6294657090004));
#34340=CARTESIAN_POINT('',(59.2229243808604,30.9911877116138,19.9294657090004));
#34341=CARTESIAN_POINT('Origin',(54.9397894030341,37.9543320991532,19.9294657090004));
#34342=CARTESIAN_POINT('',(58.9235735633387,31.1613144512955,19.6294657090004));
#34343=CARTESIAN_POINT('Ctrl Pts',(58.9235735633388,31.1613144512955,19.6294657090004));
#34344=CARTESIAN_POINT('Ctrl Pts',(59.0704513009078,31.0778410509844,19.7757724373647));
#34345=CARTESIAN_POINT('Ctrl Pts',(59.2229243808603,30.9911877116138,19.9294657090003));
#34346=CARTESIAN_POINT('',(58.9259148936722,30.8170056688373,19.9294657090004));
#34347=CARTESIAN_POINT('Ctrl Pts',(58.9259148936721,30.8170056688373,19.9294657090003));
#34348=CARTESIAN_POINT('Ctrl Pts',(58.9247223469135,30.9923778991548,19.7757724373647));
#34349=CARTESIAN_POINT('Ctrl Pts',(58.9235735633387,31.1613144512955,19.6294657090003));
#34350=CARTESIAN_POINT('',(58.6411116922923,30.6652417367664,19.9294657090004));
#34351=CARTESIAN_POINT('Origin',(54.9397894030341,37.9543320991532,19.9294657090004));
#34352=CARTESIAN_POINT('',(58.356623848585,30.8592022644217,19.6294657090004));
#34353=CARTESIAN_POINT('Ctrl Pts',(58.356623848585,30.8592022644217,19.6294657090003));
#34354=CARTESIAN_POINT('Ctrl Pts',(58.4962090055442,30.7640347158058,19.7757724373647));
#34355=CARTESIAN_POINT('Ctrl Pts',(58.6411116922923,30.6652417367664,19.9294657090003));
#34356=CARTESIAN_POINT('',(58.3308930261577,30.5158483008756,19.9294657090004));
#34357=CARTESIAN_POINT('Ctrl Pts',(58.3308930261577,30.5158483008756,19.9294657090003));
#34358=CARTESIAN_POINT('Ctrl Pts',(58.3439989123473,30.6907341981958,19.7757724373647));
#34359=CARTESIAN_POINT('Ctrl Pts',(58.356623848585,30.8592022644217,19.6294657090003));
#34360=CARTESIAN_POINT('',(58.0346673145644,30.3878034556654,19.9294657090004));
#34361=CARTESIAN_POINT('Origin',(54.9397894030341,37.9543320991532,19.9294657090004));
#34362=CARTESIAN_POINT('',(57.766935664334,30.604306995984,19.6294657090004));
#34363=CARTESIAN_POINT('Ctrl Pts',(57.766935664334,30.604306995984,19.6294657090004));
#34364=CARTESIAN_POINT('Ctrl Pts',(57.8982993244938,30.4980786233978,19.7757724373647));
#34365=CARTESIAN_POINT('Ctrl Pts',(58.0346673145644,30.3878034556654,19.9294657090003));
#34366=CARTESIAN_POINT('',(57.7133039235241,30.264192815328,19.9294657090004));
#34367=CARTESIAN_POINT('Ctrl Pts',(57.7133039235241,30.264192815328,19.9294657090004));
#34368=CARTESIAN_POINT('Ctrl Pts',(57.7406210251516,30.4374285428584,19.7757724373647));
#34369=CARTESIAN_POINT('Ctrl Pts',(57.7669356643341,30.604306995984,19.6294657090004));
#34370=CARTESIAN_POINT('',(57.4076270349543,30.1607191742974,19.9294657090004));
#34371=CARTESIAN_POINT('Origin',(54.9397894030341,37.9543320991532,19.9294657090004));
#34372=CARTESIAN_POINT('',(57.1584332881605,30.3983249319391,19.6294657090004));
#34373=CARTESIAN_POINT('Ctrl Pts',(57.1584332881605,30.3983249319391,19.6294657090003));
#34374=CARTESIAN_POINT('Ctrl Pts',(57.2807012480359,30.2817426676757,19.7757724373647));
#34375=CARTESIAN_POINT('Ctrl Pts',(57.4076270349543,30.1607191742974,19.9294657090003));
#34376=CARTESIAN_POINT('',(57.0772575393543,30.0637139379306,19.9294657090004));
#34377=CARTESIAN_POINT('Ctrl Pts',(57.0772575393543,30.0637139379306,19.9294657090004));
#34378=CARTESIAN_POINT('Ctrl Pts',(57.1186040656154,30.2341466404863,19.7757724373647));
#34379=CARTESIAN_POINT('Ctrl Pts',(57.1584332881605,30.3983249319391,19.6294657090003));
#34380=CARTESIAN_POINT('',(56.7641637030682,29.9855001010888,19.9294657090004));
#34381=CARTESIAN_POINT('Origin',(54.9397894030341,37.9543320991532,19.9294657090004));
#34382=CARTESIAN_POINT('',(56.5351662029818,30.2426268489385,19.6294657090004));
#34383=CARTESIAN_POINT('Ctrl Pts',(56.5351662029818,30.2426268489385,19.6294657090003));
#34384=CARTESIAN_POINT('Ctrl Pts',(56.6475247894728,30.1164665287319,19.7757724373647));
#34385=CARTESIAN_POINT('Ctrl Pts',(56.7641637030682,29.9855001010888,19.9294657090003));
#34386=CARTESIAN_POINT('',(56.4269866573947,29.9157458225358,19.9294657090004));
#34387=CARTESIAN_POINT('Ctrl Pts',(56.4269866573947,29.9157458225358,19.9294657090003));
#34388=CARTESIAN_POINT('Ctrl Pts',(56.4820874539788,30.0822412986007,19.7757724373647));
#34389=CARTESIAN_POINT('Ctrl Pts',(56.5351662029818,30.2426268489385,19.6294657090004));
#34390=CARTESIAN_POINT('',(56.108559461216,29.8633122900625,19.9294657090004));
#34391=CARTESIAN_POINT('Origin',(54.9397894030341,37.9543320991532,19.9294657090004));
#34392=CARTESIAN_POINT('',(55.9012821484182,30.1382488920364,19.6294657090004));
#34393=CARTESIAN_POINT('Ctrl Pts',(55.9012821484182,30.1382488920364,19.6294657090004));
#34394=CARTESIAN_POINT('Ctrl Pts',(56.0029836336694,30.0033500920025,19.7757724373647));
#34395=CARTESIAN_POINT('Ctrl Pts',(56.108559461216,29.8633122900626,19.9294657090003));
#34396=CARTESIAN_POINT('',(55.7668187230776,29.8212731725384,19.9294657090004));
#34397=CARTESIAN_POINT('Ctrl Pts',(55.7668187230776,29.8212731725384,19.9294657090004));
#34398=CARTESIAN_POINT('Ctrl Pts',(55.8353071032744,29.9827234221893,19.7757724373647));
#34399=CARTESIAN_POINT('Ctrl Pts',(55.9012821484182,30.1382488920364,19.6294657090004));
#34400=CARTESIAN_POINT('',(55.44517724746,29.7949688809415,19.9294657090004));
#34401=CARTESIAN_POINT('Origin',(54.9397894030341,37.9543320991532,19.9294657090004));
#34402=CARTESIAN_POINT('',(55.2609995182692,30.0858856793146,19.6294657090004));
#34403=CARTESIAN_POINT('Ctrl Pts',(55.2609995182692,30.0858856793146,19.6294657090003));
#34404=CARTESIAN_POINT('Ctrl Pts',(55.3513670956759,29.943146128711,19.7757724373647));
#34405=CARTESIAN_POINT('Ctrl Pts',(55.44517724746,29.7949688809415,19.9294657090003));
#34406=CARTESIAN_POINT('',(55.1011470450858,29.7809246878375,19.9294657090004));
#34407=CARTESIAN_POINT('Ctrl Pts',(55.1011470450858,29.7809246878375,19.9294657090004));
#34408=CARTESIAN_POINT('Ctrl Pts',(55.182567230025,29.9362552863001,19.7757724373647));
#34409=CARTESIAN_POINT('Ctrl Pts',(55.2609995182692,30.0858856793146,19.6294657090004));
#34410=CARTESIAN_POINT('',(54.7784317609826,29.7809246878375,19.9294657090004));
#34411=CARTESIAN_POINT('Origin',(54.9397894030341,37.9543320991532,19.9294657090004));
#34412=CARTESIAN_POINT('',(54.6185792877992,30.0858856793146,19.6294657090004));
#34413=CARTESIAN_POINT('Ctrl Pts',(54.6185792877992,30.0858856793146,19.6294657090003));
#34414=CARTESIAN_POINT('Ctrl Pts',(54.6970115760434,29.9362552863001,19.7757724373647));
#34415=CARTESIAN_POINT('Ctrl Pts',(54.7784317609826,29.7809246878375,19.9294657090003));
#34416=CARTESIAN_POINT('',(54.4344015586084,29.7949688809415,19.9294657090004));
#34417=CARTESIAN_POINT('Ctrl Pts',(54.4344015586084,29.7949688809415,19.9294657090003));
#34418=CARTESIAN_POINT('Ctrl Pts',(54.5282117103925,29.943146128711,19.7757724373647));
#34419=CARTESIAN_POINT('Ctrl Pts',(54.6185792877992,30.0858856793146,19.6294657090003));
#34420=CARTESIAN_POINT('',(54.1127600829908,29.8212731725384,19.9294657090004));
#34421=CARTESIAN_POINT('Origin',(54.9397894030341,37.9543320991532,19.9294657090004));
#34422=CARTESIAN_POINT('',(53.9782966576502,30.1382488920364,19.6294657090004));
#34423=CARTESIAN_POINT('Ctrl Pts',(53.9782966576502,30.1382488920364,19.6294657090003));
#34424=CARTESIAN_POINT('Ctrl Pts',(54.0442717027939,29.9827234221892,19.7757724373647));
#34425=CARTESIAN_POINT('Ctrl Pts',(54.1127600829908,29.8212731725384,19.9294657090003));
#34426=CARTESIAN_POINT('',(53.7710193448524,29.8633122900625,19.9294657090004));
#34427=CARTESIAN_POINT('Ctrl Pts',(53.7710193448524,29.8633122900625,19.9294657090003));
#34428=CARTESIAN_POINT('Ctrl Pts',(53.8765951723989,30.0033500920025,19.7757724373647));
#34429=CARTESIAN_POINT('Ctrl Pts',(53.9782966576502,30.1382488920364,19.6294657090003));
#34430=CARTESIAN_POINT('',(53.4525921486737,29.9157458225357,19.9294657090004));
#34431=CARTESIAN_POINT('Origin',(54.9397894030341,37.9543320991532,19.9294657090004));
#34432=CARTESIAN_POINT('',(53.3444126030865,30.2426268489385,19.6294657090004));
#34433=CARTESIAN_POINT('Ctrl Pts',(53.3444126030866,30.2426268489385,19.6294657090003));
#34434=CARTESIAN_POINT('Ctrl Pts',(53.3974913520896,30.0822412986007,19.7757724373647));
#34435=CARTESIAN_POINT('Ctrl Pts',(53.4525921486737,29.9157458225357,19.9294657090003));
#34436=CARTESIAN_POINT('',(53.1154151030002,29.9855001010888,19.9294657090004));
#34437=CARTESIAN_POINT('Ctrl Pts',(53.1154151030002,29.9855001010888,19.9294657090003));
#34438=CARTESIAN_POINT('Ctrl Pts',(53.2320540165956,30.1164665287319,19.7757724373647));
#34439=CARTESIAN_POINT('Ctrl Pts',(53.3444126030865,30.2426268489385,19.6294657090003));
#34440=CARTESIAN_POINT('',(52.8023212667141,30.0637139379306,19.9294657090004));
#34441=CARTESIAN_POINT('Origin',(54.9397894030341,37.9543320991532,19.9294657090004));
#34442=CARTESIAN_POINT('',(52.7211455179079,30.398324931939,19.6294657090004));
#34443=CARTESIAN_POINT('Ctrl Pts',(52.7211455179079,30.398324931939,19.6294657090004));
#34444=CARTESIAN_POINT('Ctrl Pts',(52.760974740453,30.2341466404863,19.7757724373647));
#34445=CARTESIAN_POINT('Ctrl Pts',(52.8023212667141,30.0637139379306,19.9294657090004));
#34446=CARTESIAN_POINT('',(52.4719517711141,30.1607191742974,19.9294657090004));
#34447=CARTESIAN_POINT('Ctrl Pts',(52.4719517711141,30.1607191742974,19.9294657090003));
#34448=CARTESIAN_POINT('Ctrl Pts',(52.5988775580325,30.2817426676756,19.7757724373647));
#34449=CARTESIAN_POINT('Ctrl Pts',(52.7211455179079,30.398324931939,19.6294657090004));
#34450=CARTESIAN_POINT('',(52.1662748825443,30.264192815328,19.9294657090004));
#34451=CARTESIAN_POINT('Origin',(54.9397894030341,37.9543320991532,19.9294657090004));
#34452=CARTESIAN_POINT('',(52.1126431417343,30.6043069959839,19.6294657090004));
#34453=CARTESIAN_POINT('Ctrl Pts',(52.1126431417343,30.6043069959839,19.6294657090004));
#34454=CARTESIAN_POINT('Ctrl Pts',(52.1389577809168,30.4374285428584,19.7757724373647));
#34455=CARTESIAN_POINT('Ctrl Pts',(52.1662748825443,30.264192815328,19.9294657090004));
#34456=CARTESIAN_POINT('',(51.8449114915039,30.3878034556653,19.9294657090004));
#34457=CARTESIAN_POINT('Ctrl Pts',(51.8449114915039,30.3878034556653,19.9294657090003));
#34458=CARTESIAN_POINT('Ctrl Pts',(51.9812794815746,30.4980786233977,19.7757724373647));
#34459=CARTESIAN_POINT('Ctrl Pts',(52.1126431417343,30.6043069959839,19.6294657090003));
#34460=CARTESIAN_POINT('',(51.5486857799107,30.5158483008756,19.9294657090004));
#34461=CARTESIAN_POINT('Origin',(54.9397894030341,37.9543320991532,19.9294657090004));
#34462=CARTESIAN_POINT('',(51.5229549574834,30.8592022644217,19.6294657090004));
#34463=CARTESIAN_POINT('Ctrl Pts',(51.5229549574834,30.8592022644216,19.6294657090004));
#34464=CARTESIAN_POINT('Ctrl Pts',(51.5355798937211,30.6907341981958,19.7757724373647));
#34465=CARTESIAN_POINT('Ctrl Pts',(51.5486857799107,30.5158483008756,19.9294657090004));
#34466=CARTESIAN_POINT('',(51.2384671137761,30.6652417367663,19.9294657090004));
#34467=CARTESIAN_POINT('Ctrl Pts',(51.2384671137761,30.6652417367663,19.9294657090003));
#34468=CARTESIAN_POINT('Ctrl Pts',(51.3833698005242,30.7640347158057,19.7757724373647));
#34469=CARTESIAN_POINT('Ctrl Pts',(51.5229549574834,30.8592022644217,19.6294657090004));
#34470=CARTESIAN_POINT('',(50.9536639123962,30.8170056688373,19.9294657090004));
#34471=CARTESIAN_POINT('Origin',(54.9397894030341,37.9543320991532,19.9294657090004));
#34472=CARTESIAN_POINT('',(50.9560052427296,31.1613144512955,19.6294657090004));
#34473=CARTESIAN_POINT('Ctrl Pts',(50.9560052427296,31.1613144512955,19.6294657090004));
#34474=CARTESIAN_POINT('Ctrl Pts',(50.9548564591548,30.9923778991548,19.7757724373647));
#34475=CARTESIAN_POINT('Ctrl Pts',(50.9536639123962,30.8170056688373,19.9294657090004));
#34476=CARTESIAN_POINT('',(50.656654425208,30.9911877116138,19.9294657090004));
#34477=CARTESIAN_POINT('Ctrl Pts',(50.656654425208,30.9911877116138,19.9294657090003));
#34478=CARTESIAN_POINT('Ctrl Pts',(50.8091275051606,31.0778410509844,19.7757724373647));
#34479=CARTESIAN_POINT('Ctrl Pts',(50.9560052427296,31.1613144512955,19.6294657090003));
#34480=CARTESIAN_POINT('',(50.3851690523575,31.1656607666167,19.9294657090004));
#34481=CARTESIAN_POINT('Origin',(54.9397894030341,37.9543320991532,19.9294657090004));
#34482=CARTESIAN_POINT('',(50.4155669542845,31.5086330498468,19.6294657090004));
#34483=CARTESIAN_POINT('Ctrl Pts',(50.4155669542845,31.5086330498468,19.6294657090003));
#34484=CARTESIAN_POINT('Ctrl Pts',(50.4006520958624,31.3403522566732,19.7757724373647));
#34485=CARTESIAN_POINT('Ctrl Pts',(50.3851690523575,31.1656607666167,19.9294657090003));
#34486=CARTESIAN_POINT('',(50.1033452932499,31.3634722635223,19.9294657090004));
#34487=CARTESIAN_POINT('Ctrl Pts',(50.1033452932499,31.3634722635223,19.9294657090003));
#34488=CARTESIAN_POINT('Ctrl Pts',(50.2623740832161,31.4374092995474,19.7757724373647));
#34489=CARTESIAN_POINT('Ctrl Pts',(50.4155669542845,31.5086330498468,19.6294657090003));
#34490=CARTESIAN_POINT('',(49.8469844392931,31.5594933520623,19.9294657090004));
#34491=CARTESIAN_POINT('Origin',(54.9397894030341,37.9543320991532,19.9294657090004));
#34492=CARTESIAN_POINT('',(49.9052366197917,31.8988467121057,19.6294657090004));
#34493=CARTESIAN_POINT('Ctrl Pts',(49.9052366197917,31.8988467121057,19.6294657090003));
#34494=CARTESIAN_POINT('Ctrl Pts',(49.8766549424443,31.7323415588134,19.7757724373647));
#34495=CARTESIAN_POINT('Ctrl Pts',(49.8469844392931,31.5594933520623,19.9294657090003));
#34496=CARTESIAN_POINT('',(49.5822218988852,31.7796179002216,19.9294657090004));
#34497=CARTESIAN_POINT('Ctrl Pts',(49.5822218988852,31.7796179002216,19.9294657090004));
#34498=CARTESIAN_POINT('Ctrl Pts',(49.7467480885058,31.8403465941252,19.7757724373647));
#34499=CARTESIAN_POINT('Ctrl Pts',(49.9052366197917,31.8988467121057,19.6294657090004));
#34500=CARTESIAN_POINT('',(49.3426916030088,31.9958825342957,19.9294657090004));
#34501=CARTESIAN_POINT('Origin',(54.9397894030341,37.9543320991532,19.9294657090004));
#34502=CARTESIAN_POINT('',(49.4284104034286,32.3293586305307,19.6294657090004));
#34503=CARTESIAN_POINT('Ctrl Pts',(49.4284104034286,32.3293586305307,19.6294657090003));
#34504=CARTESIAN_POINT('Ctrl Pts',(49.386352113503,32.1657371814434,19.7757724373647));
#34505=CARTESIAN_POINT('Ctrl Pts',(49.3426916030088,31.9958825342957,19.9294657090003));
#34506=CARTESIAN_POINT('',(49.0967522323243,32.2368552411587,19.9294657090004));
#34507=CARTESIAN_POINT('Ctrl Pts',(49.0967522323243,32.2368552411587,19.9294657090004));
#34508=CARTESIAN_POINT('Ctrl Pts',(49.2656809269522,32.2839714535024,19.7757724373647));
#34509=CARTESIAN_POINT('Ctrl Pts',(49.4284104034286,32.3293586305307,19.6294657090003));
#34510=CARTESIAN_POINT('',(48.8756465291274,32.4719242153081,19.9294657090004));
#34511=CARTESIAN_POINT('Origin',(54.9397894030341,37.9543320991532,19.9294657090004));
#34512=CARTESIAN_POINT('',(48.9882615049944,32.7973038193341,19.6294657090004));
#34513=CARTESIAN_POINT('Ctrl Pts',(48.9882615049944,32.7973038193341,19.6294657090003));
#34514=CARTESIAN_POINT('Ctrl Pts',(48.9330064934709,32.6376549481999,19.7757724373647));
#34515=CARTESIAN_POINT('Ctrl Pts',(48.8756465291274,32.4719242153081,19.9294657090004));
#34516=CARTESIAN_POINT('',(48.6501670141011,32.7321414472684,19.9294657090004));
#34517=CARTESIAN_POINT('Ctrl Pts',(48.6501670141011,32.7321414472685,19.9294657090004));
#34518=CARTESIAN_POINT('Ctrl Pts',(48.8223740211449,32.7653316274327,19.7757724373647));
#34519=CARTESIAN_POINT('Ctrl Pts',(48.9882615049944,32.7973038193341,19.6294657090003));
#34520=CARTESIAN_POINT('',(48.4489573255588,32.984450416254,19.9294657090004));
#34521=CARTESIAN_POINT('Origin',(54.9397894030341,37.9543320991532,19.9294657090004));
#34522=CARTESIAN_POINT('',(48.5877190427886,33.2995681804899,19.6294657090004));
#34523=CARTESIAN_POINT('Ctrl Pts',(48.5877190427886,33.2995681804898,19.6294657090004));
#34524=CARTESIAN_POINT('Ctrl Pts',(48.5196350226525,33.1449543242059,19.7757724373647));
#34525=CARTESIAN_POINT('Ctrl Pts',(48.4489573255588,32.984450416254,19.9294657090004));
#34526=CARTESIAN_POINT('',(48.2454381951617,33.2621804705657,19.9294657090004));
#34527=CARTESIAN_POINT('Ctrl Pts',(48.2454381951617,33.2621804705657,19.9294657090003));
#34528=CARTESIAN_POINT('Ctrl Pts',(48.4197775054016,33.2812237433775,19.7757724373647));
#34529=CARTESIAN_POINT('Ctrl Pts',(48.5877190427886,33.2995681804899,19.6294657090004));
#34530=CARTESIAN_POINT('',(48.0654635385539,33.5300503598268,19.9294657090004));
#34531=CARTESIAN_POINT('Origin',(54.9397894030341,37.9543320991532,19.9294657090004));
#34532=CARTESIAN_POINT('',(48.2294485608124,33.8328092275424,19.6294657090004));
#34533=CARTESIAN_POINT('Ctrl Pts',(48.2294485608124,33.8328092275424,19.6294657090004));
#34534=CARTESIAN_POINT('Ctrl Pts',(48.1489886199846,33.6842593158128,19.7757724373647));
#34535=CARTESIAN_POINT('Ctrl Pts',(48.0654635385539,33.5300503598268,19.9294657090004));
#34536=CARTESIAN_POINT('',(47.8852591790204,33.8234449888006,19.9294657090004));
#34537=CARTESIAN_POINT('Ctrl Pts',(47.8852591790204,33.8234449888007,19.9294657090004));
#34538=CARTESIAN_POINT('Ctrl Pts',(48.0605705931107,33.8282146244214,19.7757724373647));
#34539=CARTESIAN_POINT('Ctrl Pts',(48.2294485608124,33.8328092275424,19.6294657090004));
#34540=CARTESIAN_POINT('',(47.7277172559931,34.1050931684197,19.9294657090004));
#34541=CARTESIAN_POINT('Origin',(54.9397894030341,37.9543320991532,19.9294657090004));
#34542=CARTESIAN_POINT('',(47.9158342900129,34.393478329302,19.6294657090004));
#34543=CARTESIAN_POINT('Ctrl Pts',(47.9158342900129,34.393478329302,19.6294657090003));
#34544=CARTESIAN_POINT('Ctrl Pts',(47.8235338761247,34.2519809372803,19.7757724373647));
#34545=CARTESIAN_POINT('Ctrl Pts',(47.7277172559931,34.1050931684197,19.9294657090003));
#34546=CARTESIAN_POINT('',(47.5720268976044,34.4121998792066,19.9294657090004));
#34547=CARTESIAN_POINT('Ctrl Pts',(47.5720268976044,34.4121998792066,19.9294657090004));
#34548=CARTESIAN_POINT('Ctrl Pts',(47.7471437470088,34.4026641364982,19.7757724373647));
#34549=CARTESIAN_POINT('Ctrl Pts',(47.9158342900129,34.393478329302,19.6294657090004));
#34550=CARTESIAN_POINT('',(47.4379661236627,34.7057520270169,19.9294657090004));
#34551=CARTESIAN_POINT('Origin',(54.9397894030341,37.9543320991532,19.9294657090004));
#34552=CARTESIAN_POINT('',(47.6489632816196,34.9778443254006,19.6294657090004));
#34553=CARTESIAN_POINT('Ctrl Pts',(47.6489632816196,34.9778443254005,19.6294657090003));
#34554=CARTESIAN_POINT('Ctrl Pts',(47.5454366386968,34.8443410948852,19.7757724373647));
#34555=CARTESIAN_POINT('Ctrl Pts',(47.4379661236628,34.7057520270169,19.9294657090003));
#34556=CARTESIAN_POINT('',(47.3078258600668,35.0245270751256,19.9294657090004));
#34557=CARTESIAN_POINT('Ctrl Pts',(47.3078258600668,35.0245270751256,19.9294657090003));
#34558=CARTESIAN_POINT('Ctrl Pts',(47.4815827710446,35.0007494128825,19.7757724373647));
#34559=CARTESIAN_POINT('Ctrl Pts',(47.6489632816196,34.9778443254006,19.6294657090004));
#34560=CARTESIAN_POINT('',(47.1981383875429,35.3280296500161,19.9294657090004));
#34561=CARTESIAN_POINT('Origin',(54.9397894030341,37.9543320991532,19.9294657090004));
#34562=CARTESIAN_POINT('',(47.4306115181626,35.5820183565475,19.6294657090004));
#34563=CARTESIAN_POINT('Ctrl Pts',(47.4306115181626,35.5820183565475,19.6294657090004));
#34564=CARTESIAN_POINT('Ctrl Pts',(47.3165475989333,35.4573977295111,19.7757724373647));
#34565=CARTESIAN_POINT('Ctrl Pts',(47.1981383875429,35.3280296500162,19.9294657090004));
#34566=CARTESIAN_POINT('',(47.0944142807223,35.6563516400958,19.9294657090004));
#34567=CARTESIAN_POINT('Ctrl Pts',(47.0944142807223,35.6563516400958,19.9294657090004));
#34568=CARTESIAN_POINT('Ctrl Pts',(47.2656549296989,35.6184902947371,19.7757724373647));
#34569=CARTESIAN_POINT('Ctrl Pts',(47.4306115181626,35.5820183565475,19.6294657090004));
#34570=CARTESIAN_POINT('',(47.0098300616486,35.967784882505,19.9294657090004));
#34571=CARTESIAN_POINT('Origin',(54.9397894030341,37.9543320991532,19.9294657090004));
#34572=CARTESIAN_POINT('',(47.2622320946023,36.2019797442472,19.6294657090004));
#34573=CARTESIAN_POINT('Ctrl Pts',(47.2622320946023,36.2019797442472,19.6294657090003));
#34574=CARTESIAN_POINT('Ctrl Pts',(47.1383899756297,36.0870710504017,19.7757724373647));
#34575=CARTESIAN_POINT('Ctrl Pts',(47.0098300616486,35.967784882505,19.9294657090003));
#34576=CARTESIAN_POINT('',(46.9332123784209,36.3034688858808,19.9294657090004));
#34577=CARTESIAN_POINT('Ctrl Pts',(46.9332123784209,36.3034688858808,19.9294657090004));
#34578=CARTESIAN_POINT('Ctrl Pts',(47.1007971871301,36.2517758184133,19.7757724373647));
#34579=CARTESIAN_POINT('Ctrl Pts',(47.2622320946023,36.2019797442472,19.6294657090004));
#34580=CARTESIAN_POINT('',(46.8742943068201,36.6207602589635,19.9294657090004));
#34581=CARTESIAN_POINT('Origin',(54.9397894030341,37.9543320991532,19.9294657090004));
#34582=CARTESIAN_POINT('',(47.1449455482218,36.8336027477511,19.6294657090004));
#34583=CARTESIAN_POINT('Ctrl Pts',(47.1449455482218,36.8336027477511,19.6294657090003));
#34584=CARTESIAN_POINT('Ctrl Pts',(47.0121493783752,36.7291706854955,19.7757724373647));
#34585=CARTESIAN_POINT('Ctrl Pts',(46.8742943068201,36.6207602589635,19.9294657090003));
#34586=CARTESIAN_POINT('',(46.8252929252262,36.961572353977,19.9294657090004));
#34587=CARTESIAN_POINT('Ctrl Pts',(46.8252929252262,36.961572353977,19.9294657090004));
#34588=CARTESIAN_POINT('Ctrl Pts',(46.9881066444156,36.8963915732357,19.7757724373647));
#34589=CARTESIAN_POINT('Ctrl Pts',(47.1449455482218,36.8336027477511,19.6294657090003));
#34590=CARTESIAN_POINT('',(46.7924330911438,37.2826103359946,19.9294657090004));
#34591=CARTESIAN_POINT('Origin',(54.9397894030341,37.9543320991532,19.9294657090004));
#34592=CARTESIAN_POINT('',(47.0795324016364,37.4726840201812,19.6294657090004));
#34593=CARTESIAN_POINT('Ctrl Pts',(47.0795324016364,37.4726840201812,19.6294657090004));
#34594=CARTESIAN_POINT('Ctrl Pts',(46.9386659175162,37.3794235676597,19.7757724373647));
#34595=CARTESIAN_POINT('Ctrl Pts',(46.7924330911438,37.2826103359945,19.9294657090004));
#34596=CARTESIAN_POINT('',(46.7713741072936,37.6262824743834,19.9294657090004));
#34597=CARTESIAN_POINT('Ctrl Pts',(46.7713741072936,37.6262824743834,19.9294657090004));
#34598=CARTESIAN_POINT('Ctrl Pts',(46.9283332385243,37.5480477477103,19.7757724373647));
#34599=CARTESIAN_POINT('Ctrl Pts',(47.0795324016364,37.4726840201812,19.6294657090004));
#34600=CARTESIAN_POINT('',(46.764791187504,37.9489306105331,19.9294657090004));
#34601=CARTESIAN_POINT('Origin',(54.9397894030341,37.9543320991532,19.9294657090004));
#34602=CARTESIAN_POINT('',(46.7746038105401,37.9543320991532,19.9196513014945));
#34603=CARTESIAN_POINT('Ctrl Pts',(46.764791187504,37.9489306105331,19.9294657090004));
#34604=CARTESIAN_POINT('Ctrl Pts',(46.7697004459005,37.9516329769915,19.924554666134));
#34605=CARTESIAN_POINT('Ctrl Pts',(46.7746038105401,37.9543320991532,19.9196513014945));
#34606=CARTESIAN_POINT('',(47.1647894030341,37.9543320991532,19.5294657090004));
#34607=CARTESIAN_POINT('',(46.7647894030341,37.9543320991532,19.9294657090004));
#34608=CARTESIAN_POINT('Origin',(54.9397894030341,37.9543320991532,19.5294657090004));
#34609=CARTESIAN_POINT('',(47.0664279685441,38.1149705811105,19.6294657090004));
#34610=CARTESIAN_POINT('Ctrl Pts',(46.7746038105401,37.9543320991532,19.9196513014945));
#34611=CARTESIAN_POINT('Ctrl Pts',(46.9231556085686,38.0361044085143,19.7710995034659));
#34612=CARTESIAN_POINT('Ctrl Pts',(47.0664279685441,38.1149705811105,19.6294657090004));
#34613=CARTESIAN_POINT('',(46.7718147454605,38.2931757109183,19.9294657090004));
#34614=CARTESIAN_POINT('Ctrl Pts',(46.7718147454605,38.2931757109183,19.9294657090004));
#34615=CARTESIAN_POINT('Ctrl Pts',(46.9218747516106,38.2024076775116,19.7757724373647));
#34616=CARTESIAN_POINT('Ctrl Pts',(47.0664279685441,38.1149705811105,19.6294657090004));
#34617=CARTESIAN_POINT('',(46.7915525482088,38.6152868310873,19.9294657090004));
#34618=CARTESIAN_POINT('Origin',(54.9397894030341,37.9543320991532,19.9294657090004));
#34619=CARTESIAN_POINT('',(47.1057194567852,38.7561881194459,19.6294657090004));
#34620=CARTESIAN_POINT('Ctrl Pts',(47.1057194567852,38.7561881194459,19.6294657090004));
#34621=CARTESIAN_POINT('Ctrl Pts',(46.9515721418295,38.6870543097372,19.7757724373647));
#34622=CARTESIAN_POINT('Ctrl Pts',(46.7915525482088,38.6152868310873,19.9294657090003));
#34623=CARTESIAN_POINT('',(46.8266119073525,38.9578139991222,19.9294657090004));
#34624=CARTESIAN_POINT('Ctrl Pts',(46.8266119073525,38.9578139991222,19.9294657090004));
#34625=CARTESIAN_POINT('Ctrl Pts',(46.9687741638393,38.8551167052684,19.7757724373647));
#34626=CARTESIAN_POINT('Ctrl Pts',(47.1057194567852,38.7561881194459,19.6294657090003));
#34627=CARTESIAN_POINT('',(46.872539080818,39.2772445069503,19.9294657090004));
#34628=CARTESIAN_POINT('Origin',(54.9397894030341,37.9543320991532,19.9294657090004));
#34629=CARTESIAN_POINT('',(47.197145387988,39.3920694382632,19.6294657090004));
#34630=CARTESIAN_POINT('Ctrl Pts',(47.1971453879881,39.3920694382632,19.6294657090004));
#34631=CARTESIAN_POINT('Ctrl Pts',(47.0378759382084,39.3357301028059,19.7757724373647));
#34632=CARTESIAN_POINT('Ctrl Pts',(46.872539080818,39.2772445069503,19.9294657090004));
#34633=CARTESIAN_POINT('',(46.9354009268983,39.6157742808447,19.9294657090004));
#34634=CARTESIAN_POINT('Ctrl Pts',(46.9354009268983,39.6157742808447,19.9294657090004));
#34635=CARTESIAN_POINT('Ctrl Pts',(47.0687193673599,39.5018311600905,19.7757724373647));
#34636=CARTESIAN_POINT('Ctrl Pts',(47.197145387988,39.3920694382632,19.6294657090004));
#34637=CARTESIAN_POINT('',(47.0072118333189,39.9303984190046,19.9294657090004));
#34638=CARTESIAN_POINT('Origin',(54.9397894030341,37.9543320991532,19.9294657090004));
#34639=CARTESIAN_POINT('',(47.3400973376647,40.0183828522986,19.6294657090004));
#34640=CARTESIAN_POINT('Ctrl Pts',(47.3400973376646,40.0183828522986,19.6294657090004));
#34641=CARTESIAN_POINT('Ctrl Pts',(47.1767656649717,39.9752129200749,19.7757724373647));
#34642=CARTESIAN_POINT('Ctrl Pts',(47.0072118333189,39.9303984190046,19.9294657090004));
#34643=CARTESIAN_POINT('',(47.0974578311216,40.2626779389666,19.9294657090004));
#34644=CARTESIAN_POINT('Ctrl Pts',(47.0974578311216,40.2626779389666,19.9294657090004));
#34645=CARTESIAN_POINT('Ctrl Pts',(47.2210452433328,40.1382472639815,19.7757724373647));
#34646=CARTESIAN_POINT('Ctrl Pts',(47.3400973376647,40.0183828522986,19.6294657090004));
#34647=CARTESIAN_POINT('',(47.1946745807631,40.5704019357283,19.9294657090004));
#34648=CARTESIAN_POINT('Origin',(54.9397894030341,37.9543320991532,19.9294657090004));
#34649=CARTESIAN_POINT('',(47.5336239841754,40.6309603491163,19.6294657090004));
#34650=CARTESIAN_POINT('Ctrl Pts',(47.5336239841753,40.6309603491163,19.6294657090004));
#34651=CARTESIAN_POINT('Ctrl Pts',(47.367317033903,40.6012471089026,19.7757724373647));
#34652=CARTESIAN_POINT('Ctrl Pts',(47.1946745807631,40.5704019357283,19.9294657090003));
#34653=CARTESIAN_POINT('',(47.3117041580624,40.8942199363749,19.9294657090004));
#34654=CARTESIAN_POINT('Ctrl Pts',(47.3117041580624,40.8942199363749,19.9294657090004));
#34655=CARTESIAN_POINT('Ctrl Pts',(47.4247380881853,40.7601297727712,19.7757724373647));
#34656=CARTESIAN_POINT('Ctrl Pts',(47.5336239841754,40.6309603491163,19.6294657090004));
#34657=CARTESIAN_POINT('',(47.4336797894956,41.1929959393107,19.9294657090004));
#34658=CARTESIAN_POINT('Origin',(54.9397894030341,37.9543320991532,19.9294657090004));
#34659=CARTESIAN_POINT('',(47.7764374396173,41.2257253265431,19.6294657090004));
#34660=CARTESIAN_POINT('Ctrl Pts',(47.7764374396173,41.2257253265431,19.6294657090004));
#34661=CARTESIAN_POINT('Ctrl Pts',(47.6082619570809,41.2096665150506,19.7757724373647));
#34662=CARTESIAN_POINT('Ctrl Pts',(47.4336797894956,41.1929959393107,19.9294657090003));
#34663=CARTESIAN_POINT('',(47.5767141337629,41.5061974652738,19.9294657090004));
#34664=CARTESIAN_POINT('Ctrl Pts',(47.5767141337629,41.5061974652738,19.9294657090004));
#34665=CARTESIAN_POINT('Ctrl Pts',(47.678442359642,41.363340160967,19.7757724373647));
#34666=CARTESIAN_POINT('Ctrl Pts',(47.7764374396173,41.2257253265431,19.6294657090004));
#34667=CARTESIAN_POINT('',(47.7226369192852,41.7940371693788,19.9294657090004));
#34668=CARTESIAN_POINT('Origin',(54.9397894030341,37.9543320991532,19.9294657090004));
#34669=CARTESIAN_POINT('',(48.0669218205059,41.7987197217834,19.6294657090004));
#34670=CARTESIAN_POINT('Ctrl Pts',(48.0669218205059,41.7987197217834,19.6294657090004));
#34671=CARTESIAN_POINT('Ctrl Pts',(47.8979969857948,41.7964222077531,19.7757724373647));
#34672=CARTESIAN_POINT('Ctrl Pts',(47.7226369192852,41.7940371693788,19.9294657090004));
#34673=CARTESIAN_POINT('',(47.8907241605586,42.0945379161777,19.9294657090004));
#34674=CARTESIAN_POINT('Ctrl Pts',(47.8907241605586,42.0945379161777,19.9294657090003));
#34675=CARTESIAN_POINT('Ctrl Pts',(47.9804696976346,41.9438641629582,19.7757724373647));
#34676=CARTESIAN_POINT('Ctrl Pts',(48.0669218205059,41.7987197217834,19.6294657090004));
#34677=CARTESIAN_POINT('',(48.0596230081078,42.3695257957113,19.9294657090004));
#34678=CARTESIAN_POINT('Origin',(54.9397894030341,37.9543320991532,19.9294657090004));
#34679=CARTESIAN_POINT('',(48.4031440012129,42.3461303516745,19.6294657090004));
#34680=CARTESIAN_POINT('Ctrl Pts',(48.4031440012129,42.3461303516745,19.6294657090003));
#34681=CARTESIAN_POINT('Ctrl Pts',(48.2345939812314,42.3576094246832,19.7757724373647));
#34682=CARTESIAN_POINT('Ctrl Pts',(48.0596230081078,42.3695257957113,19.9294657090003));
#34683=CARTESIAN_POINT('',(48.251644553529,42.6553259804552,19.9294657090004));
#34684=CARTESIAN_POINT('Ctrl Pts',(48.251644553529,42.6553259804552,19.9294657090004));
#34685=CARTESIAN_POINT('Ctrl Pts',(48.3288101600596,42.4978384872912,19.7757724373647));
#34686=CARTESIAN_POINT('Ctrl Pts',(48.4031440012129,42.3461303516745,19.6294657090004));
#34687=CARTESIAN_POINT('',(48.4423954691411,42.9156320364489,19.9294657090004));
#34688=CARTESIAN_POINT('Origin',(54.9397894030341,37.9543320991532,19.9294657090004));
#34689=CARTESIAN_POINT('',(48.7828664785984,42.8643142887907,19.6294657090004));
#34690=CARTESIAN_POINT('Ctrl Pts',(48.7828664785984,42.8643142887908,19.6294657090004));
#34691=CARTESIAN_POINT('Ctrl Pts',(48.6158129459207,42.8894935575015,19.7757724373647));
#34692=CARTESIAN_POINT('Ctrl Pts',(48.4423954691411,42.9156320364489,19.9294657090003));
#34693=CARTESIAN_POINT('',(48.6570734470067,43.184829706062,19.9294657090004));
#34694=CARTESIAN_POINT('Ctrl Pts',(48.6570734470067,43.184829706062,19.9294657090003));
#34695=CARTESIAN_POINT('Ctrl Pts',(48.7211455986118,43.0215765262369,19.7757724373647));
#34696=CARTESIAN_POINT('Ctrl Pts',(48.7828664785984,42.8643142887907,19.6294657090003));
#34697=CARTESIAN_POINT('',(48.8684070148099,43.4287216446606,19.9294657090004));
#34698=CARTESIAN_POINT('Origin',(54.9397894030341,37.9543320991532,19.9294657090004));
#34699=CARTESIAN_POINT('',(49.2035622622253,43.349823104525,19.6294657090004));
#34700=CARTESIAN_POINT('Ctrl Pts',(49.2035622622253,43.349823104525,19.6294657090004));
#34701=CARTESIAN_POINT('Ctrl Pts',(49.0391169305495,43.3885350050588,19.7757724373647));
#34702=CARTESIAN_POINT('Ctrl Pts',(48.8684070148099,43.4287216446606,19.9294657090004));
#34703=CARTESIAN_POINT('',(49.1043127785965,43.6795253330662,19.9294657090004));
#34704=CARTESIAN_POINT('Ctrl Pts',(49.1043127785966,43.6795253330662,19.9294657090004));
#34705=CARTESIAN_POINT('Ctrl Pts',(49.1548650856785,43.5115928895569,19.7757724373647));
#34706=CARTESIAN_POINT('Ctrl Pts',(49.2035622622253,43.349823104525,19.6294657090004));
#34707=CARTESIAN_POINT('',(49.3348226085648,43.9053800936577,19.9294657090004));
#34708=CARTESIAN_POINT('Origin',(54.9397894030341,37.9543320991532,19.9294657090004));
#34709=CARTESIAN_POINT('',(49.6624316910633,43.7994258178118,19.6294657090004));
#34710=CARTESIAN_POINT('Ctrl Pts',(49.6624316910633,43.7994258178118,19.6294657090004));
#34711=CARTESIAN_POINT('Ctrl Pts',(49.5016889169402,43.8514127288577,19.7757724373647));
#34712=CARTESIAN_POINT('Ctrl Pts',(49.3348226085648,43.9053800936577,19.9294657090003));
#34713=CARTESIAN_POINT('',(49.5903862443362,44.1361207436891,19.9294657090004));
#34714=CARTESIAN_POINT('Ctrl Pts',(49.5903862443362,44.136120743689,19.9294657090004));
#34715=CARTESIAN_POINT('Ctrl Pts',(49.6270822896318,43.9646265992002,19.7757724373647));
#34716=CARTESIAN_POINT('Ctrl Pts',(49.6624316910633,43.7994258178118,19.6294657090004));
#34717=CARTESIAN_POINT('',(49.8385383315824,44.3424353001052,19.9294657090004));
#34718=CARTESIAN_POINT('Origin',(54.9397894030341,37.9543320991532,19.9294657090004));
#34719=CARTESIAN_POINT('',(50.1564210647719,44.2101303967736,19.6294657090004));
#34720=CARTESIAN_POINT('Ctrl Pts',(50.1564210647719,44.2101303967736,19.6294657090003));
#34721=CARTESIAN_POINT('Ctrl Pts',(50.0004505648425,44.2750463540157,19.7757724373647));
#34722=CARTESIAN_POINT('Ctrl Pts',(49.8385383315824,44.3424353001052,19.9294657090004));
#34723=CARTESIAN_POINT('',(50.1120591055075,44.5515773708059,19.9294657090004));
#34724=CARTESIAN_POINT('Ctrl Pts',(50.1120591055075,44.5515773708059,19.9294657090004));
#34725=CARTESIAN_POINT('Ctrl Pts',(50.1346546828898,44.3776627905745,19.7757724373647));
#34726=CARTESIAN_POINT('Ctrl Pts',(50.1564210647719,44.2101303967736,19.6294657090004));
#34727=CARTESIAN_POINT('',(50.3762020388334,44.7369787337131,19.9294657090004));
#34728=CARTESIAN_POINT('Origin',(54.9397894030341,37.9543320991532,19.9294657090004));
#34729=CARTESIAN_POINT('',(50.6822429655713,44.5792036701988,19.6294657090004));
#34730=CARTESIAN_POINT('Ctrl Pts',(50.6822429655713,44.5792036701988,19.6294657090004));
#34731=CARTESIAN_POINT('Ctrl Pts',(50.5320826977793,44.6566166686521,19.7757724373647));
#34732=CARTESIAN_POINT('Ctrl Pts',(50.3762020388334,44.7369787337131,19.9294657090004));
#34733=CARTESIAN_POINT('',(50.6658597152895,44.9231304191087,19.9294657090004));
#34734=CARTESIAN_POINT('Ctrl Pts',(50.6658597152895,44.9231304191087,19.9294657090004));
#34735=CARTESIAN_POINT('Ctrl Pts',(50.674204454919,44.7479527759724,19.7757724373647));
#34736=CARTESIAN_POINT('Ctrl Pts',(50.6822429655713,44.5792036701988,19.6294657090004));
#34737=CARTESIAN_POINT('',(50.9442356670542,45.086384773026,19.9294657090004));
#34738=CARTESIAN_POINT('Origin',(54.9397894030341,37.9543320991532,19.9294657090004));
#34739=CARTESIAN_POINT('',(51.2363981354663,44.9041895163455,19.6294657090004));
#34740=CARTESIAN_POINT('Ctrl Pts',(51.2363981354663,44.9041895163455,19.6294657090004));
#34741=CARTESIAN_POINT('Ctrl Pts',(51.0930473916193,44.9935843852776,19.7757724373647));
#34742=CARTESIAN_POINT('Ctrl Pts',(50.9442356670542,45.0863847730261,19.9294657090004));
#34743=CARTESIAN_POINT('',(51.2481026219946,45.2483072643631,19.9294657090004));
#34744=CARTESIAN_POINT('Ctrl Pts',(51.2481026219946,45.2483072643631,19.9294657090004));
#34745=CARTESIAN_POINT('Ctrl Pts',(51.2421409910059,45.0730323366345,19.7757724373647));
#34746=CARTESIAN_POINT('Ctrl Pts',(51.2363981354663,44.9041895163455,19.6294657090003));
#34747=CARTESIAN_POINT('',(51.5388590461679,45.3883281785002,19.9294657090004));
#34748=CARTESIAN_POINT('Origin',(54.9397894030341,37.9543320991532,19.9294657090004));
#34749=CARTESIAN_POINT('',(51.8151987632305,45.1829252080266,19.6294657090004));
#34750=CARTESIAN_POINT('Ctrl Pts',(51.8151987632305,45.1829252080266,19.6294657090003));
#34751=CARTESIAN_POINT('Ctrl Pts',(51.6796115188774,45.2837070393337,19.7757724373647));
#34752=CARTESIAN_POINT('Ctrl Pts',(51.538859046168,45.3883281785002,19.9294657090003));
#34753=CARTESIAN_POINT('',(51.8549130951421,45.5249439083141,19.9294657090004));
#34754=CARTESIAN_POINT('Ctrl Pts',(51.8549130951421,45.5249439083141,19.9294657090004));
#34755=CARTESIAN_POINT('Ctrl Pts',(51.8346847672058,45.3507381217191,19.7757724373647));
#34756=CARTESIAN_POINT('Ctrl Pts',(51.8151987632305,45.1829252080266,19.6294657090004));
#34757=CARTESIAN_POINT('',(52.1561150556927,45.6407995665893,19.9294657090004));
#34758=CARTESIAN_POINT('Origin',(54.9397894030341,37.9543320991532,19.9294657090004));
#34759=CARTESIAN_POINT('',(52.4147930261813,45.413555805202,19.6294657090004));
#34760=CARTESIAN_POINT('Ctrl Pts',(52.4147930261813,45.413555805202,19.6294657090003));
#34761=CARTESIAN_POINT('Ctrl Pts',(52.2878715920631,45.5250539124247,19.7757724373647));
#34762=CARTESIAN_POINT('Ctrl Pts',(52.1561150556927,45.6407995665893,19.9294657090004));
#34763=CARTESIAN_POINT('',(52.4822529111499,45.7511993797382,19.9294657090004));
#34764=CARTESIAN_POINT('Ctrl Pts',(52.4822529111499,45.7511993797382,19.9294657090003));
#34765=CARTESIAN_POINT('Ctrl Pts',(52.447892502451,45.5792220450446,19.7757724373647));
#34766=CARTESIAN_POINT('Ctrl Pts',(52.4147930261813,45.413555805202,19.6294657090003));
#34767=CARTESIAN_POINT('',(52.791895958725,45.8421187818605,19.9294657090004));
#34768=CARTESIAN_POINT('Origin',(54.9397894030341,37.9543320991532,19.9294657090004));
#34769=CARTESIAN_POINT('',(53.0311907234251,45.594546499299,19.6294657090004));
#34770=CARTESIAN_POINT('Ctrl Pts',(53.0311907234251,45.594546499299,19.6294657090003));
#34771=CARTESIAN_POINT('Ctrl Pts',(52.9137797407451,45.7160188809296,19.7757724373647));
#34772=CARTESIAN_POINT('Ctrl Pts',(52.791895958725,45.8421187818605,19.9294657090003));
#34773=CARTESIAN_POINT('',(53.1259472270462,45.9255679858026,19.9294657090004));
#34774=CARTESIAN_POINT('Ctrl Pts',(53.1259472270462,45.9255679858026,19.9294657090004));
#34775=CARTESIAN_POINT('Ctrl Pts',(53.0776834004354,45.7569635837984,19.7757724373647));
#34776=CARTESIAN_POINT('Ctrl Pts',(53.0311907234251,45.594546499299,19.6294657090004));
#34777=CARTESIAN_POINT('',(53.4419707382517,45.9909460781514,19.9294657090004));
#34778=CARTESIAN_POINT('Origin',(54.9397894030341,37.9543320991532,19.9294657090004));
#34779=CARTESIAN_POINT('',(53.660289829985,45.7246928271096,19.6294657090004));
#34780=CARTESIAN_POINT('Ctrl Pts',(53.660289829985,45.7246928271096,19.6294657090003));
#34781=CARTESIAN_POINT('Ctrl Pts',(53.5531706494617,45.8553311044899,19.7757724373647));
#34782=CARTESIAN_POINT('Ctrl Pts',(53.4419707382517,45.9909460781514,19.9294657090003));
#34783=CARTESIAN_POINT('',(53.7817123633608,46.0468893322027,19.9294657090004));
#34784=CARTESIAN_POINT('Ctrl Pts',(53.7817123633608,46.0468893322027,19.9294657090003));
#34785=CARTESIAN_POINT('Ctrl Pts',(53.7198663066414,45.8827798973656,19.7757724373647));
#34786=CARTESIAN_POINT('Ctrl Pts',(53.660289829985,45.7246928271096,19.6294657090003));
#34787=CARTESIAN_POINT('',(54.1020132538699,46.0862910343601,19.9294657090004));
#34788=CARTESIAN_POINT('Origin',(54.9397894030341,37.9543320991532,19.9294657090004));
#34789=CARTESIAN_POINT('',(54.297903795101,45.803128686295,19.6294657090004));
#34790=CARTESIAN_POINT('Ctrl Pts',(54.297903795101,45.803128686295,19.6294657090004));
#34791=CARTESIAN_POINT('Ctrl Pts',(54.2017892772072,45.9420634832428,19.7757724373647));
#34792=CARTESIAN_POINT('Ctrl Pts',(54.1020132538699,46.0862910343602,19.9294657090004));
#34793=CARTESIAN_POINT('',(54.4451843113051,46.1143560453948,19.9294657090004));
#34794=CARTESIAN_POINT('Ctrl Pts',(54.4451843113051,46.1143560453948,19.9294657090003));
#34795=CARTESIAN_POINT('Ctrl Pts',(54.3701675997806,45.9558336989374,19.7757724373647));
#34796=CARTESIAN_POINT('Ctrl Pts',(54.297903795101,45.803128686295,19.6294657090003));
#34797=CARTESIAN_POINT('',(54.7676310315374,46.1275191455338,19.9294657090004));
#34798=CARTESIAN_POINT('Origin',(54.9397894030341,37.9543320991532,19.9294657090004));
#34799=CARTESIAN_POINT('',(54.9397894030341,45.8293320991532,19.6294657090004));
#34800=CARTESIAN_POINT('Ctrl Pts',(54.9397894030341,45.8293320991532,19.6294657090003));
#34801=CARTESIAN_POINT('Ctrl Pts',(54.8553191740287,45.9756388275175,19.7757724373647));
#34802=CARTESIAN_POINT('Ctrl Pts',(54.7676310315374,46.1275191455338,19.9294657090003));
#34803=CARTESIAN_POINT('',(55.1119477745308,46.1275191455338,19.9294657090004));
#34804=CARTESIAN_POINT('Ctrl Pts',(55.1119477745308,46.1275191455338,19.9294657090003));
#34805=CARTESIAN_POINT('Ctrl Pts',(55.0242596320395,45.9756388275175,19.7757724373647));
#34806=CARTESIAN_POINT('Ctrl Pts',(54.9397894030341,45.8293320991532,19.6294657090003));
#34807=CARTESIAN_POINT('',(55.434394494763,46.1143560453948,19.9294657090004));
#34808=CARTESIAN_POINT('Origin',(54.9397894030341,37.9543320991532,19.9294657090004));
#34809=CARTESIAN_POINT('',(55.5816750109672,45.803128686295,19.6294657090004));
#34810=CARTESIAN_POINT('Ctrl Pts',(55.5816750109672,45.803128686295,19.6294657090004));
#34811=CARTESIAN_POINT('Ctrl Pts',(55.5094112062876,45.9558336989374,19.7757724373647));
#34812=CARTESIAN_POINT('Ctrl Pts',(55.434394494763,46.1143560453948,19.9294657090003));
#34813=CARTESIAN_POINT('',(55.7775655521983,46.0862910343602,19.9294657090004));
#34814=CARTESIAN_POINT('Ctrl Pts',(55.7775655521983,46.0862910343601,19.9294657090004));
#34815=CARTESIAN_POINT('Ctrl Pts',(55.6777895288609,45.9420634832429,19.7757724373647));
#34816=CARTESIAN_POINT('Ctrl Pts',(55.5816750109672,45.803128686295,19.6294657090003));
#34817=CARTESIAN_POINT('',(56.0978664427074,46.0468893322027,19.9294657090004));
#34818=CARTESIAN_POINT('Origin',(54.9397894030341,37.9543320991532,19.9294657090004));
#34819=CARTESIAN_POINT('',(56.2192889760832,45.7246928271096,19.6294657090004));
#34820=CARTESIAN_POINT('Ctrl Pts',(56.2192889760832,45.7246928271096,19.6294657090004));
#34821=CARTESIAN_POINT('Ctrl Pts',(56.1597124994268,45.8827798973656,19.7757724373647));
#34822=CARTESIAN_POINT('Ctrl Pts',(56.0978664427074,46.0468893322027,19.9294657090004));
#34823=CARTESIAN_POINT('',(56.4376080678164,45.9909460781515,19.9294657090004));
#34824=CARTESIAN_POINT('Ctrl Pts',(56.4376080678164,45.9909460781515,19.9294657090004));
#34825=CARTESIAN_POINT('Ctrl Pts',(56.3264081566065,45.85533110449,19.7757724373647));
#34826=CARTESIAN_POINT('Ctrl Pts',(56.2192889760832,45.7246928271096,19.6294657090004));
#34827=CARTESIAN_POINT('',(56.753631579022,45.9255679858027,19.9294657090004));
#34828=CARTESIAN_POINT('Origin',(54.9397894030341,37.9543320991532,19.9294657090004));
#34829=CARTESIAN_POINT('',(56.8483880826431,45.594546499299,19.6294657090004));
#34830=CARTESIAN_POINT('Ctrl Pts',(56.8483880826431,45.594546499299,19.6294657090003));
#34831=CARTESIAN_POINT('Ctrl Pts',(56.8018954056327,45.7569635837985,19.7757724373647));
#34832=CARTESIAN_POINT('Ctrl Pts',(56.753631579022,45.9255679858026,19.9294657090003));
#34833=CARTESIAN_POINT('',(57.0876828473432,45.8421187818605,19.9294657090004));
#34834=CARTESIAN_POINT('Ctrl Pts',(57.0876828473432,45.8421187818605,19.9294657090003));
#34835=CARTESIAN_POINT('Ctrl Pts',(56.965799065323,45.7160188809296,19.7757724373647));
#34836=CARTESIAN_POINT('Ctrl Pts',(56.8483880826431,45.594546499299,19.6294657090003));
#34837=CARTESIAN_POINT('',(57.3973258949183,45.7511993797383,19.9294657090004));
#34838=CARTESIAN_POINT('Origin',(54.9397894030341,37.9543320991532,19.9294657090004));
#34839=CARTESIAN_POINT('',(57.4647857798868,45.413555805202,19.6294657090004));
#34840=CARTESIAN_POINT('Ctrl Pts',(57.4647857798868,45.413555805202,19.6294657090003));
#34841=CARTESIAN_POINT('Ctrl Pts',(57.4316863036172,45.5792220450446,19.7757724373647));
#34842=CARTESIAN_POINT('Ctrl Pts',(57.3973258949183,45.7511993797383,19.9294657090003));
#34843=CARTESIAN_POINT('',(57.7234637503755,45.6407995665893,19.9294657090004));
#34844=CARTESIAN_POINT('Ctrl Pts',(57.7234637503755,45.6407995665893,19.9294657090004));
#34845=CARTESIAN_POINT('Ctrl Pts',(57.5917072140051,45.5250539124248,19.7757724373647));
#34846=CARTESIAN_POINT('Ctrl Pts',(57.4647857798868,45.413555805202,19.6294657090003));
#34847=CARTESIAN_POINT('',(58.024665710926,45.5249439083142,19.9294657090004));
#34848=CARTESIAN_POINT('Origin',(54.9397894030341,37.9543320991532,19.9294657090004));
#34849=CARTESIAN_POINT('',(58.0643800428377,45.1829252080266,19.6294657090004));
#34850=CARTESIAN_POINT('Ctrl Pts',(58.0643800428377,45.1829252080266,19.6294657090004));
#34851=CARTESIAN_POINT('Ctrl Pts',(58.0448940388624,45.3507381217191,19.7757724373647));
#34852=CARTESIAN_POINT('Ctrl Pts',(58.024665710926,45.5249439083142,19.9294657090003));
#34853=CARTESIAN_POINT('',(58.3407197599002,45.3883281785002,19.9294657090004));
#34854=CARTESIAN_POINT('Ctrl Pts',(58.3407197599002,45.3883281785002,19.9294657090003));
#34855=CARTESIAN_POINT('Ctrl Pts',(58.1999672871908,45.2837070393338,19.7757724373647));
#34856=CARTESIAN_POINT('Ctrl Pts',(58.0643800428377,45.1829252080266,19.6294657090003));
#34857=CARTESIAN_POINT('',(58.6314761840736,45.2483072643631,19.9294657090004));
#34858=CARTESIAN_POINT('Origin',(54.9397894030341,37.9543320991532,19.9294657090004));
#34859=CARTESIAN_POINT('',(58.6431806706019,44.9041895163456,19.6294657090004));
#34860=CARTESIAN_POINT('Ctrl Pts',(58.6431806706019,44.9041895163456,19.6294657090004));
#34861=CARTESIAN_POINT('Ctrl Pts',(58.6374378150623,45.0730323366346,19.7757724373647));
#34862=CARTESIAN_POINT('Ctrl Pts',(58.6314761840736,45.2483072643631,19.9294657090003));
#34863=CARTESIAN_POINT('',(58.935343139014,45.0863847730261,19.9294657090004));
#34864=CARTESIAN_POINT('Ctrl Pts',(58.935343139014,45.0863847730261,19.9294657090003));
#34865=CARTESIAN_POINT('Ctrl Pts',(58.7865314144489,44.9935843852776,19.7757724373647));
#34866=CARTESIAN_POINT('Ctrl Pts',(58.6431806706019,44.9041895163456,19.6294657090004));
#34867=CARTESIAN_POINT('',(59.2137190907787,44.9231304191088,19.9294657090004));
#34868=CARTESIAN_POINT('Origin',(54.9397894030341,37.9543320991532,19.9294657090004));
#34869=CARTESIAN_POINT('',(59.1973358404969,44.5792036701988,19.6294657090004));
#34870=CARTESIAN_POINT('Ctrl Pts',(59.1973358404969,44.5792036701988,19.6294657090003));
#34871=CARTESIAN_POINT('Ctrl Pts',(59.2053743511492,44.7479527759724,19.7757724373647));
#34872=CARTESIAN_POINT('Ctrl Pts',(59.2137190907787,44.9231304191088,19.9294657090003));
#34873=CARTESIAN_POINT('',(59.5033767672348,44.7369787337132,19.9294657090004));
#34874=CARTESIAN_POINT('Ctrl Pts',(59.5033767672348,44.7369787337132,19.9294657090003));
#34875=CARTESIAN_POINT('Ctrl Pts',(59.3474961082889,44.6566166686521,19.7757724373647));
#34876=CARTESIAN_POINT('Ctrl Pts',(59.1973358404969,44.5792036701988,19.6294657090003));
#34877=CARTESIAN_POINT('',(59.7675197005607,44.551577370806,19.9294657090004));
#34878=CARTESIAN_POINT('Origin',(54.9397894030341,37.9543320991532,19.9294657090004));
#34879=CARTESIAN_POINT('',(59.7231577412963,44.2101303967737,19.6294657090004));
#34880=CARTESIAN_POINT('Ctrl Pts',(59.7231577412963,44.2101303967737,19.6294657090003));
#34881=CARTESIAN_POINT('Ctrl Pts',(59.7449241231784,44.3776627905746,19.7757724373647));
#34882=CARTESIAN_POINT('Ctrl Pts',(59.7675197005607,44.551577370806,19.9294657090003));
#34883=CARTESIAN_POINT('',(60.0410404744858,44.3424353001052,19.9294657090004));
#34884=CARTESIAN_POINT('Ctrl Pts',(60.0410404744858,44.3424353001052,19.9294657090003));
#34885=CARTESIAN_POINT('Ctrl Pts',(59.8791282412257,44.2750463540158,19.7757724373647));
#34886=CARTESIAN_POINT('Ctrl Pts',(59.7231577412963,44.2101303967737,19.6294657090003));
#34887=CARTESIAN_POINT('',(60.289192561732,44.1361207436891,19.9294657090004));
#34888=CARTESIAN_POINT('Origin',(54.9397894030341,37.9543320991532,19.9294657090004));
#34889=CARTESIAN_POINT('',(60.2171471150049,43.7994258178119,19.6294657090004));
#34890=CARTESIAN_POINT('Ctrl Pts',(60.2171471150049,43.7994258178119,19.6294657090003));
#34891=CARTESIAN_POINT('Ctrl Pts',(60.2524965164364,43.9646265992003,19.7757724373647));
#34892=CARTESIAN_POINT('Ctrl Pts',(60.289192561732,44.1361207436891,19.9294657090004));
#34893=CARTESIAN_POINT('',(60.5447561975034,43.9053800936578,19.9294657090004));
#34894=CARTESIAN_POINT('Ctrl Pts',(60.5447561975034,43.9053800936578,19.9294657090003));
#34895=CARTESIAN_POINT('Ctrl Pts',(60.377889889128,43.8514127288578,19.7757724373647));
#34896=CARTESIAN_POINT('Ctrl Pts',(60.2171471150048,43.7994258178119,19.6294657090003));
#34897=CARTESIAN_POINT('',(60.7752660274717,43.6795253330662,19.9294657090004));
#34898=CARTESIAN_POINT('Origin',(54.9397894030341,37.9543320991532,19.9294657090004));
#34899=CARTESIAN_POINT('',(60.6760165438429,43.3498231045251,19.6294657090004));
#34900=CARTESIAN_POINT('Ctrl Pts',(60.6760165438429,43.3498231045251,19.6294657090004));
#34901=CARTESIAN_POINT('Ctrl Pts',(60.7247137203897,43.511592889557,19.7757724373647));
#34902=CARTESIAN_POINT('Ctrl Pts',(60.7752660274716,43.6795253330662,19.9294657090004));
#34903=CARTESIAN_POINT('',(61.0111717912583,43.4287216446607,19.9294657090004));
#34904=CARTESIAN_POINT('Ctrl Pts',(61.0111717912583,43.4287216446607,19.9294657090003));
#34905=CARTESIAN_POINT('Ctrl Pts',(60.8404618755187,43.3885350050589,19.7757724373647));
#34906=CARTESIAN_POINT('Ctrl Pts',(60.6760165438429,43.3498231045251,19.6294657090003));
#34907=CARTESIAN_POINT('',(61.2225053590615,43.184829706062,19.9294657090004));
#34908=CARTESIAN_POINT('Origin',(54.9397894030341,37.9543320991532,19.9294657090004));
#34909=CARTESIAN_POINT('',(61.0967123274698,42.8643142887908,19.6294657090004));
#34910=CARTESIAN_POINT('Ctrl Pts',(61.0967123274698,42.8643142887908,19.6294657090004));
#34911=CARTESIAN_POINT('Ctrl Pts',(61.1584332074564,43.021576526237,19.7757724373647));
#34912=CARTESIAN_POINT('Ctrl Pts',(61.2225053590615,43.184829706062,19.9294657090003));
#34913=CARTESIAN_POINT('',(61.4371833369271,42.915632036449,19.9294657090004));
#34914=CARTESIAN_POINT('Ctrl Pts',(61.4371833369271,42.915632036449,19.9294657090004));
#34915=CARTESIAN_POINT('Ctrl Pts',(61.2637658601475,42.8894935575016,19.7757724373647));
#34916=CARTESIAN_POINT('Ctrl Pts',(61.0967123274698,42.8643142887908,19.6294657090003));
#34917=CARTESIAN_POINT('',(61.6279342525392,42.6553259804552,19.9294657090004));
#34918=CARTESIAN_POINT('Origin',(54.9397894030341,37.9543320991532,19.9294657090004));
#34919=CARTESIAN_POINT('',(61.4764348048553,42.3461303516746,19.6294657090004));
#34920=CARTESIAN_POINT('Ctrl Pts',(61.4764348048554,42.3461303516746,19.6294657090003));
#34921=CARTESIAN_POINT('Ctrl Pts',(61.5507686460086,42.4978384872913,19.7757724373647));
#34922=CARTESIAN_POINT('Ctrl Pts',(61.6279342525392,42.6553259804552,19.9294657090003));
#34923=CARTESIAN_POINT('',(61.8199557979604,42.3695257957114,19.9294657090004));
#34924=CARTESIAN_POINT('Ctrl Pts',(61.8199557979604,42.3695257957114,19.9294657090004));
#34925=CARTESIAN_POINT('Ctrl Pts',(61.6449848248368,42.3576094246833,19.7757724373647));
#34926=CARTESIAN_POINT('Ctrl Pts',(61.4764348048553,42.3461303516746,19.6294657090003));
#34927=CARTESIAN_POINT('',(61.9888546455096,42.0945379161778,19.9294657090004));
#34928=CARTESIAN_POINT('Origin',(54.9397894030341,37.9543320991532,19.9294657090004));
#34929=CARTESIAN_POINT('',(61.8126569855623,41.7987197217835,19.6294657090004));
#34930=CARTESIAN_POINT('Ctrl Pts',(61.8126569855623,41.7987197217835,19.6294657090004));
#34931=CARTESIAN_POINT('Ctrl Pts',(61.8991091084337,41.9438641629583,19.7757724373647));
#34932=CARTESIAN_POINT('Ctrl Pts',(61.9888546455096,42.0945379161778,19.9294657090003));
#34933=CARTESIAN_POINT('',(62.1569418867831,41.7940371693789,19.9294657090004));
#34934=CARTESIAN_POINT('Ctrl Pts',(62.156941886783,41.7940371693789,19.9294657090003));
#34935=CARTESIAN_POINT('Ctrl Pts',(61.9815818202734,41.7964222077532,19.7757724373647));
#34936=CARTESIAN_POINT('Ctrl Pts',(61.8126569855623,41.7987197217835,19.6294657090003));
#34937=CARTESIAN_POINT('',(62.3028646723053,41.5061974652739,19.9294657090004));
#34938=CARTESIAN_POINT('Origin',(54.9397894030341,37.9543320991532,19.9294657090004));
#34939=CARTESIAN_POINT('',(62.1031413664509,41.2257253265432,19.6294657090004));
#34940=CARTESIAN_POINT('Ctrl Pts',(62.1031413664509,41.2257253265432,19.6294657090004));
#34941=CARTESIAN_POINT('Ctrl Pts',(62.2011364464262,41.3633401609671,19.7757724373647));
#34942=CARTESIAN_POINT('Ctrl Pts',(62.3028646723053,41.5061974652739,19.9294657090004));
#34943=CARTESIAN_POINT('',(62.4458990165727,41.1929959393108,19.9294657090004));
#34944=CARTESIAN_POINT('Ctrl Pts',(62.4458990165727,41.1929959393108,19.9294657090003));
#34945=CARTESIAN_POINT('Ctrl Pts',(62.2713168489873,41.2096665150507,19.7757724373647));
#34946=CARTESIAN_POINT('Ctrl Pts',(62.1031413664509,41.2257253265432,19.6294657090003));
#34947=CARTESIAN_POINT('',(62.5678746480059,40.894219936375,19.9294657090004));
#34948=CARTESIAN_POINT('Origin',(54.9397894030341,37.9543320991532,19.9294657090004));
#34949=CARTESIAN_POINT('',(62.3459548218929,40.6309603491164,19.6294657090004));
#34950=CARTESIAN_POINT('Ctrl Pts',(62.3459548218929,40.6309603491164,19.6294657090004));
#34951=CARTESIAN_POINT('Ctrl Pts',(62.4548407178829,40.7601297727713,19.7757724373647));
#34952=CARTESIAN_POINT('Ctrl Pts',(62.5678746480059,40.894219936375,19.9294657090004));
#34953=CARTESIAN_POINT('',(62.6849042253051,40.5704019357284,19.9294657090004));
#34954=CARTESIAN_POINT('Ctrl Pts',(62.6849042253051,40.5704019357284,19.9294657090004));
#34955=CARTESIAN_POINT('Ctrl Pts',(62.5122617721652,40.6012471089027,19.7757724373647));
#34956=CARTESIAN_POINT('Ctrl Pts',(62.3459548218929,40.6309603491164,19.6294657090004));
#34957=CARTESIAN_POINT('',(62.7821209749467,40.2626779389667,19.9294657090004));
#34958=CARTESIAN_POINT('Origin',(54.9397894030341,37.9543320991532,19.9294657090004));
#34959=CARTESIAN_POINT('',(62.5394814684036,40.0183828522987,19.6294657090004));
#34960=CARTESIAN_POINT('Ctrl Pts',(62.5394814684036,40.0183828522987,19.6294657090003));
#34961=CARTESIAN_POINT('Ctrl Pts',(62.6585335627355,40.1382472639816,19.7757724373647));
#34962=CARTESIAN_POINT('Ctrl Pts',(62.7821209749466,40.2626779389667,19.9294657090004));
#34963=CARTESIAN_POINT('',(62.8723669727493,39.9303984190047,19.9294657090004));
#34964=CARTESIAN_POINT('Ctrl Pts',(62.8723669727493,39.9303984190047,19.9294657090003));
#34965=CARTESIAN_POINT('Ctrl Pts',(62.7028131410966,39.9752129200751,19.7757724373647));
#34966=CARTESIAN_POINT('Ctrl Pts',(62.5394814684036,40.0183828522987,19.6294657090003));
#34967=CARTESIAN_POINT('',(62.94417787917,39.6157742808448,19.9294657090004));
#34968=CARTESIAN_POINT('Origin',(54.9397894030341,37.9543320991532,19.9294657090004));
#34969=CARTESIAN_POINT('',(62.6824334180802,39.3920694382633,19.6294657090004));
#34970=CARTESIAN_POINT('Ctrl Pts',(62.6824334180802,39.3920694382633,19.6294657090003));
#34971=CARTESIAN_POINT('Ctrl Pts',(62.8108594387083,39.5018311600907,19.7757724373647));
#34972=CARTESIAN_POINT('Ctrl Pts',(62.94417787917,39.6157742808448,19.9294657090003));
#34973=CARTESIAN_POINT('',(63.0070397252503,39.2772445069504,19.9294657090004));
#34974=CARTESIAN_POINT('Ctrl Pts',(63.0070397252503,39.2772445069504,19.9294657090004));
#34975=CARTESIAN_POINT('Ctrl Pts',(62.8417028678599,39.335730102806,19.7757724373647));
#34976=CARTESIAN_POINT('Ctrl Pts',(62.6824334180802,39.3920694382633,19.6294657090003));
#34977=CARTESIAN_POINT('',(63.0529668987158,38.9578139991223,19.9294657090004));
#34978=CARTESIAN_POINT('Origin',(54.9397894030341,37.9543320991532,19.9294657090004));
#34979=CARTESIAN_POINT('',(62.773859349283,38.756188119446,19.6294657090004));
#34980=CARTESIAN_POINT('Ctrl Pts',(62.773859349283,38.756188119446,19.6294657090003));
#34981=CARTESIAN_POINT('Ctrl Pts',(62.910804642229,38.8551167052685,19.7757724373647));
#34982=CARTESIAN_POINT('Ctrl Pts',(63.0529668987157,38.9578139991223,19.9294657090004));
#34983=CARTESIAN_POINT('',(63.0880262578595,38.6152868310874,19.9294657090004));
#34984=CARTESIAN_POINT('Ctrl Pts',(63.0880262578595,38.6152868310874,19.9294657090003));
#34985=CARTESIAN_POINT('Ctrl Pts',(62.9280066642388,38.6870543097374,19.7757724373647));
#34986=CARTESIAN_POINT('Ctrl Pts',(62.773859349283,38.756188119446,19.6294657090004));
#34987=CARTESIAN_POINT('',(63.1077640606078,38.2931757109184,19.9294657090004));
#34988=CARTESIAN_POINT('Origin',(54.9397894030341,37.9543320991532,19.9294657090004));
#34989=CARTESIAN_POINT('Ctrl Pts',(62.8131508375241,38.1149705811106,19.6294657090003));
#34990=CARTESIAN_POINT('Ctrl Pts',(62.9577040544577,38.2024076775117,19.7757724373647));
#34991=CARTESIAN_POINT('Ctrl Pts',(63.1077640606078,38.2931757109184,19.9294657090003));
#34992=CARTESIAN_POINT('Origin',(54.9397894030341,37.9543320991532,22.6294657090004));
#34993=CARTESIAN_POINT('',(47.0664279685441,38.1149705811105,22.9294657090004));
#34994=CARTESIAN_POINT('',(46.764791187504,37.9489306105331,22.6294657090004));
#34995=CARTESIAN_POINT('Ctrl Pts',(46.764791187504,37.9489306105332,22.6294657090004));
#34996=CARTESIAN_POINT('Ctrl Pts',(46.9184286133609,38.0335023712478,22.783158980636));
#34997=CARTESIAN_POINT('Ctrl Pts',(47.0664279685441,38.1149705811105,22.9294657090004));
#34998=CARTESIAN_POINT('',(46.7713741072936,37.6262824743834,22.6294657090004));
#34999=CARTESIAN_POINT('Origin',(54.9397894030341,37.9543320991532,22.6294657090004));
#35000=CARTESIAN_POINT('',(47.0795324016364,37.4726840201812,22.9294657090004));
#35001=CARTESIAN_POINT('Ctrl Pts',(46.7713741072936,37.6262824743834,22.6294657090004));
#35002=CARTESIAN_POINT('Ctrl Pts',(46.9283332385242,37.5480477477103,22.783158980636));
#35003=CARTESIAN_POINT('Ctrl Pts',(47.0795324016364,37.4726840201812,22.9294657090004));
#35004=CARTESIAN_POINT('',(46.7924330911438,37.2826103359946,22.6294657090004));
#35005=CARTESIAN_POINT('Ctrl Pts',(47.0795324016364,37.4726840201812,22.9294657090003));
#35006=CARTESIAN_POINT('Ctrl Pts',(46.9386659175162,37.3794235676597,22.783158980636));
#35007=CARTESIAN_POINT('Ctrl Pts',(46.7924330911438,37.2826103359945,22.6294657090004));
#35008=CARTESIAN_POINT('',(46.8252929252262,36.961572353977,22.6294657090004));
#35009=CARTESIAN_POINT('Origin',(54.9397894030341,37.9543320991532,22.6294657090004));
#35010=CARTESIAN_POINT('',(47.1449455482218,36.8336027477511,22.9294657090004));
#35011=CARTESIAN_POINT('Ctrl Pts',(46.8252929252262,36.961572353977,22.6294657090004));
#35012=CARTESIAN_POINT('Ctrl Pts',(46.9881066444155,36.8963915732357,22.783158980636));
#35013=CARTESIAN_POINT('Ctrl Pts',(47.1449455482218,36.8336027477511,22.9294657090004));
#35014=CARTESIAN_POINT('',(46.8742943068201,36.6207602589635,22.6294657090004));
#35015=CARTESIAN_POINT('Ctrl Pts',(47.1449455482218,36.8336027477511,22.9294657090004));
#35016=CARTESIAN_POINT('Ctrl Pts',(47.0121493783752,36.7291706854955,22.783158980636));
#35017=CARTESIAN_POINT('Ctrl Pts',(46.8742943068201,36.6207602589635,22.6294657090004));
#35018=CARTESIAN_POINT('',(46.9332123784209,36.3034688858808,22.6294657090004));
#35019=CARTESIAN_POINT('Origin',(54.9397894030341,37.9543320991532,22.6294657090004));
#35020=CARTESIAN_POINT('',(47.2622320946023,36.2019797442472,22.9294657090004));
#35021=CARTESIAN_POINT('Ctrl Pts',(46.9332123784209,36.3034688858808,22.6294657090004));
#35022=CARTESIAN_POINT('Ctrl Pts',(47.1007971871301,36.2517758184132,22.783158980636));
#35023=CARTESIAN_POINT('Ctrl Pts',(47.2622320946023,36.2019797442472,22.9294657090004));
#35024=CARTESIAN_POINT('',(47.0098300616486,35.967784882505,22.6294657090004));
#35025=CARTESIAN_POINT('Ctrl Pts',(47.2622320946023,36.2019797442472,22.9294657090004));
#35026=CARTESIAN_POINT('Ctrl Pts',(47.1383899756297,36.0870710504017,22.7831589806361));
#35027=CARTESIAN_POINT('Ctrl Pts',(47.0098300616486,35.967784882505,22.6294657090004));
#35028=CARTESIAN_POINT('',(47.0944142807223,35.6563516400958,22.6294657090004));
#35029=CARTESIAN_POINT('Origin',(54.9397894030341,37.9543320991532,22.6294657090004));
#35030=CARTESIAN_POINT('',(47.4306115181626,35.5820183565475,22.9294657090004));
#35031=CARTESIAN_POINT('Ctrl Pts',(47.0944142807223,35.6563516400958,22.6294657090004));
#35032=CARTESIAN_POINT('Ctrl Pts',(47.2656549296989,35.6184902947371,22.783158980636));
#35033=CARTESIAN_POINT('Ctrl Pts',(47.4306115181626,35.5820183565475,22.9294657090004));
#35034=CARTESIAN_POINT('',(47.1981383875429,35.3280296500161,22.6294657090004));
#35035=CARTESIAN_POINT('Ctrl Pts',(47.4306115181626,35.5820183565475,22.9294657090004));
#35036=CARTESIAN_POINT('Ctrl Pts',(47.3165475989333,35.4573977295111,22.783158980636));
#35037=CARTESIAN_POINT('Ctrl Pts',(47.1981383875429,35.3280296500161,22.6294657090004));
#35038=CARTESIAN_POINT('',(47.3078258600668,35.0245270751256,22.6294657090004));
#35039=CARTESIAN_POINT('Origin',(54.9397894030341,37.9543320991532,22.6294657090004));
#35040=CARTESIAN_POINT('',(47.6489632816196,34.9778443254006,22.9294657090004));
#35041=CARTESIAN_POINT('Ctrl Pts',(47.3078258600668,35.0245270751256,22.6294657090004));
#35042=CARTESIAN_POINT('Ctrl Pts',(47.4815827710446,35.0007494128825,22.783158980636));
#35043=CARTESIAN_POINT('Ctrl Pts',(47.6489632816196,34.9778443254006,22.9294657090004));
#35044=CARTESIAN_POINT('',(47.4379661236627,34.7057520270169,22.6294657090004));
#35045=CARTESIAN_POINT('Ctrl Pts',(47.6489632816196,34.9778443254006,22.9294657090004));
#35046=CARTESIAN_POINT('Ctrl Pts',(47.5454366386968,34.8443410948852,22.7831589806361));
#35047=CARTESIAN_POINT('Ctrl Pts',(47.4379661236628,34.7057520270169,22.6294657090004));
#35048=CARTESIAN_POINT('',(47.5720268976044,34.4121998792066,22.6294657090004));
#35049=CARTESIAN_POINT('Origin',(54.9397894030341,37.9543320991532,22.6294657090004));
#35050=CARTESIAN_POINT('',(47.9158342900129,34.393478329302,22.9294657090004));
#35051=CARTESIAN_POINT('Ctrl Pts',(47.5720268976044,34.4121998792066,22.6294657090004));
#35052=CARTESIAN_POINT('Ctrl Pts',(47.7471437470088,34.4026641364982,22.783158980636));
#35053=CARTESIAN_POINT('Ctrl Pts',(47.9158342900129,34.393478329302,22.9294657090004));
#35054=CARTESIAN_POINT('',(47.7277172559931,34.1050931684197,22.6294657090004));
#35055=CARTESIAN_POINT('Ctrl Pts',(47.9158342900129,34.393478329302,22.9294657090004));
#35056=CARTESIAN_POINT('Ctrl Pts',(47.8235338761247,34.2519809372803,22.783158980636));
#35057=CARTESIAN_POINT('Ctrl Pts',(47.7277172559931,34.1050931684197,22.6294657090004));
#35058=CARTESIAN_POINT('',(47.8852591790204,33.8234449888006,22.6294657090004));
#35059=CARTESIAN_POINT('Origin',(54.9397894030341,37.9543320991532,22.6294657090004));
#35060=CARTESIAN_POINT('',(48.2294485608124,33.8328092275424,22.9294657090004));
#35061=CARTESIAN_POINT('Ctrl Pts',(47.8852591790204,33.8234449888007,22.6294657090004));
#35062=CARTESIAN_POINT('Ctrl Pts',(48.0605705931107,33.8282146244214,22.783158980636));
#35063=CARTESIAN_POINT('Ctrl Pts',(48.2294485608124,33.8328092275424,22.9294657090004));
#35064=CARTESIAN_POINT('',(48.0654635385539,33.5300503598268,22.6294657090004));
#35065=CARTESIAN_POINT('Ctrl Pts',(48.2294485608124,33.8328092275424,22.9294657090004));
#35066=CARTESIAN_POINT('Ctrl Pts',(48.1489886199846,33.6842593158128,22.783158980636));
#35067=CARTESIAN_POINT('Ctrl Pts',(48.0654635385539,33.5300503598268,22.6294657090004));
#35068=CARTESIAN_POINT('',(48.2454381951617,33.2621804705657,22.6294657090004));
#35069=CARTESIAN_POINT('Origin',(54.9397894030341,37.9543320991532,22.6294657090004));
#35070=CARTESIAN_POINT('',(48.5877190427886,33.2995681804899,22.9294657090004));
#35071=CARTESIAN_POINT('Ctrl Pts',(48.2454381951617,33.2621804705657,22.6294657090004));
#35072=CARTESIAN_POINT('Ctrl Pts',(48.4197775054016,33.2812237433775,22.783158980636));
#35073=CARTESIAN_POINT('Ctrl Pts',(48.5877190427886,33.2995681804899,22.9294657090004));
#35074=CARTESIAN_POINT('',(48.4489573255588,32.984450416254,22.6294657090004));
#35075=CARTESIAN_POINT('Ctrl Pts',(48.5877190427886,33.2995681804899,22.9294657090004));
#35076=CARTESIAN_POINT('Ctrl Pts',(48.5196350226525,33.1449543242059,22.783158980636));
#35077=CARTESIAN_POINT('Ctrl Pts',(48.4489573255588,32.984450416254,22.6294657090004));
#35078=CARTESIAN_POINT('',(48.6501670141011,32.7321414472684,22.6294657090004));
#35079=CARTESIAN_POINT('Origin',(54.9397894030341,37.9543320991532,22.6294657090004));
#35080=CARTESIAN_POINT('',(48.9882615049944,32.7973038193341,22.9294657090004));
#35081=CARTESIAN_POINT('Ctrl Pts',(48.6501670141012,32.7321414472685,22.6294657090004));
#35082=CARTESIAN_POINT('Ctrl Pts',(48.8223740211449,32.7653316274327,22.783158980636));
#35083=CARTESIAN_POINT('Ctrl Pts',(48.9882615049944,32.7973038193341,22.9294657090004));
#35084=CARTESIAN_POINT('',(48.8756465291274,32.4719242153081,22.6294657090004));
#35085=CARTESIAN_POINT('Ctrl Pts',(48.9882615049944,32.7973038193341,22.9294657090004));
#35086=CARTESIAN_POINT('Ctrl Pts',(48.9330064934709,32.6376549481999,22.7831589806361));
#35087=CARTESIAN_POINT('Ctrl Pts',(48.8756465291274,32.4719242153081,22.6294657090004));
#35088=CARTESIAN_POINT('',(49.0967522323243,32.2368552411587,22.6294657090004));
#35089=CARTESIAN_POINT('Origin',(54.9397894030341,37.9543320991532,22.6294657090004));
#35090=CARTESIAN_POINT('',(49.4284104034286,32.3293586305307,22.9294657090004));
#35091=CARTESIAN_POINT('Ctrl Pts',(49.0967522323243,32.2368552411587,22.6294657090004));
#35092=CARTESIAN_POINT('Ctrl Pts',(49.2656809269522,32.2839714535024,22.783158980636));
#35093=CARTESIAN_POINT('Ctrl Pts',(49.4284104034286,32.3293586305307,22.9294657090004));
#35094=CARTESIAN_POINT('',(49.3426916030088,31.9958825342957,22.6294657090004));
#35095=CARTESIAN_POINT('Ctrl Pts',(49.4284104034286,32.3293586305307,22.9294657090004));
#35096=CARTESIAN_POINT('Ctrl Pts',(49.386352113503,32.1657371814434,22.7831589806361));
#35097=CARTESIAN_POINT('Ctrl Pts',(49.3426916030088,31.9958825342957,22.6294657090004));
#35098=CARTESIAN_POINT('',(49.5822218988852,31.7796179002216,22.6294657090004));
#35099=CARTESIAN_POINT('Origin',(54.9397894030341,37.9543320991532,22.6294657090004));
#35100=CARTESIAN_POINT('',(49.9052366197917,31.8988467121057,22.9294657090004));
#35101=CARTESIAN_POINT('Ctrl Pts',(49.5822218988853,31.7796179002216,22.6294657090004));
#35102=CARTESIAN_POINT('Ctrl Pts',(49.7467480885058,31.8403465941252,22.7831589806361));
#35103=CARTESIAN_POINT('Ctrl Pts',(49.9052366197917,31.8988467121057,22.9294657090004));
#35104=CARTESIAN_POINT('',(49.8469844392931,31.5594933520623,22.6294657090004));
#35105=CARTESIAN_POINT('Ctrl Pts',(49.9052366197917,31.8988467121057,22.9294657090004));
#35106=CARTESIAN_POINT('Ctrl Pts',(49.8766549424443,31.7323415588134,22.783158980636));
#35107=CARTESIAN_POINT('Ctrl Pts',(49.8469844392932,31.5594933520623,22.6294657090004));
#35108=CARTESIAN_POINT('',(50.1033452932499,31.3634722635223,22.6294657090004));
#35109=CARTESIAN_POINT('Origin',(54.9397894030341,37.9543320991532,22.6294657090004));
#35110=CARTESIAN_POINT('',(50.4155669542845,31.5086330498468,22.9294657090004));
#35111=CARTESIAN_POINT('Ctrl Pts',(50.1033452932499,31.3634722635223,22.6294657090004));
#35112=CARTESIAN_POINT('Ctrl Pts',(50.2623740832161,31.4374092995474,22.783158980636));
#35113=CARTESIAN_POINT('Ctrl Pts',(50.4155669542845,31.5086330498468,22.9294657090004));
#35114=CARTESIAN_POINT('',(50.3851690523575,31.1656607666167,22.6294657090004));
#35115=CARTESIAN_POINT('Ctrl Pts',(50.4155669542845,31.5086330498468,22.9294657090004));
#35116=CARTESIAN_POINT('Ctrl Pts',(50.4006520958624,31.3403522566732,22.7831589806361));
#35117=CARTESIAN_POINT('Ctrl Pts',(50.3851690523575,31.1656607666167,22.6294657090004));
#35118=CARTESIAN_POINT('',(50.656654425208,30.9911877116138,22.6294657090004));
#35119=CARTESIAN_POINT('Origin',(54.9397894030341,37.9543320991532,22.6294657090004));
#35120=CARTESIAN_POINT('',(50.9560052427296,31.1613144512955,22.9294657090004));
#35121=CARTESIAN_POINT('Ctrl Pts',(50.656654425208,30.9911877116138,22.6294657090004));
#35122=CARTESIAN_POINT('Ctrl Pts',(50.8091275051606,31.0778410509844,22.783158980636));
#35123=CARTESIAN_POINT('Ctrl Pts',(50.9560052427296,31.1613144512955,22.9294657090004));
#35124=CARTESIAN_POINT('',(50.9536639123962,30.8170056688373,22.6294657090004));
#35125=CARTESIAN_POINT('Ctrl Pts',(50.9560052427296,31.1613144512955,22.9294657090004));
#35126=CARTESIAN_POINT('Ctrl Pts',(50.9548564591548,30.9923778991548,22.783158980636));
#35127=CARTESIAN_POINT('Ctrl Pts',(50.9536639123962,30.8170056688373,22.6294657090004));
#35128=CARTESIAN_POINT('',(51.2384671137761,30.6652417367663,22.6294657090004));
#35129=CARTESIAN_POINT('Origin',(54.9397894030341,37.9543320991532,22.6294657090004));
#35130=CARTESIAN_POINT('',(51.5229549574834,30.8592022644217,22.9294657090004));
#35131=CARTESIAN_POINT('Ctrl Pts',(51.2384671137761,30.6652417367663,22.6294657090004));
#35132=CARTESIAN_POINT('Ctrl Pts',(51.3833698005242,30.7640347158057,22.783158980636));
#35133=CARTESIAN_POINT('Ctrl Pts',(51.5229549574834,30.8592022644216,22.9294657090004));
#35134=CARTESIAN_POINT('',(51.5486857799107,30.5158483008756,22.6294657090004));
#35135=CARTESIAN_POINT('Ctrl Pts',(51.5229549574834,30.8592022644217,22.9294657090004));
#35136=CARTESIAN_POINT('Ctrl Pts',(51.5355798937211,30.6907341981958,22.783158980636));
#35137=CARTESIAN_POINT('Ctrl Pts',(51.5486857799107,30.5158483008756,22.6294657090004));
#35138=CARTESIAN_POINT('',(51.844911491504,30.3878034556653,22.6294657090004));
#35139=CARTESIAN_POINT('Origin',(54.9397894030341,37.9543320991532,22.6294657090004));
#35140=CARTESIAN_POINT('',(52.1126431417343,30.6043069959839,22.9294657090004));
#35141=CARTESIAN_POINT('Ctrl Pts',(51.8449114915039,30.3878034556653,22.6294657090004));
#35142=CARTESIAN_POINT('Ctrl Pts',(51.9812794815746,30.4980786233977,22.7831589806361));
#35143=CARTESIAN_POINT('Ctrl Pts',(52.1126431417343,30.6043069959839,22.9294657090004));
#35144=CARTESIAN_POINT('',(52.1662748825443,30.264192815328,22.6294657090004));
#35145=CARTESIAN_POINT('Ctrl Pts',(52.1126431417343,30.6043069959839,22.9294657090004));
#35146=CARTESIAN_POINT('Ctrl Pts',(52.1389577809168,30.4374285428584,22.783158980636));
#35147=CARTESIAN_POINT('Ctrl Pts',(52.1662748825443,30.264192815328,22.6294657090004));
#35148=CARTESIAN_POINT('',(52.4719517711141,30.1607191742974,22.6294657090004));
#35149=CARTESIAN_POINT('Origin',(54.9397894030341,37.9543320991532,22.6294657090004));
#35150=CARTESIAN_POINT('',(52.7211455179079,30.398324931939,22.9294657090004));
#35151=CARTESIAN_POINT('Ctrl Pts',(52.4719517711141,30.1607191742974,22.6294657090004));
#35152=CARTESIAN_POINT('Ctrl Pts',(52.5988775580325,30.2817426676756,22.7831589806361));
#35153=CARTESIAN_POINT('Ctrl Pts',(52.7211455179079,30.398324931939,22.9294657090004));
#35154=CARTESIAN_POINT('',(52.8023212667141,30.0637139379306,22.6294657090004));
#35155=CARTESIAN_POINT('Ctrl Pts',(52.7211455179079,30.398324931939,22.9294657090004));
#35156=CARTESIAN_POINT('Ctrl Pts',(52.760974740453,30.2341466404863,22.783158980636));
#35157=CARTESIAN_POINT('Ctrl Pts',(52.8023212667141,30.0637139379306,22.6294657090004));
#35158=CARTESIAN_POINT('',(53.1154151030002,29.9855001010888,22.6294657090004));
#35159=CARTESIAN_POINT('Origin',(54.9397894030341,37.9543320991532,22.6294657090004));
#35160=CARTESIAN_POINT('',(53.3444126030865,30.2426268489385,22.9294657090004));
#35161=CARTESIAN_POINT('Ctrl Pts',(53.1154151030002,29.9855001010888,22.6294657090004));
#35162=CARTESIAN_POINT('Ctrl Pts',(53.2320540165956,30.1164665287319,22.783158980636));
#35163=CARTESIAN_POINT('Ctrl Pts',(53.3444126030865,30.2426268489385,22.9294657090004));
#35164=CARTESIAN_POINT('',(53.4525921486737,29.9157458225357,22.6294657090004));
#35165=CARTESIAN_POINT('Ctrl Pts',(53.3444126030866,30.2426268489385,22.9294657090004));
#35166=CARTESIAN_POINT('Ctrl Pts',(53.3974913520896,30.0822412986007,22.7831589806361));
#35167=CARTESIAN_POINT('Ctrl Pts',(53.4525921486737,29.9157458225357,22.6294657090004));
#35168=CARTESIAN_POINT('',(53.7710193448524,29.8633122900625,22.6294657090004));
#35169=CARTESIAN_POINT('Origin',(54.9397894030341,37.9543320991532,22.6294657090004));
#35170=CARTESIAN_POINT('',(53.9782966576502,30.1382488920364,22.9294657090004));
#35171=CARTESIAN_POINT('Ctrl Pts',(53.7710193448524,29.8633122900625,22.6294657090004));
#35172=CARTESIAN_POINT('Ctrl Pts',(53.876595172399,30.0033500920025,22.783158980636));
#35173=CARTESIAN_POINT('Ctrl Pts',(53.9782966576502,30.1382488920364,22.9294657090004));
#35174=CARTESIAN_POINT('',(54.1127600829908,29.8212731725384,22.6294657090004));
#35175=CARTESIAN_POINT('Ctrl Pts',(53.9782966576502,30.1382488920364,22.9294657090004));
#35176=CARTESIAN_POINT('Ctrl Pts',(54.044271702794,29.9827234221892,22.7831589806361));
#35177=CARTESIAN_POINT('Ctrl Pts',(54.1127600829908,29.8212731725384,22.6294657090004));
#35178=CARTESIAN_POINT('',(54.4344015586084,29.7949688809415,22.6294657090004));
#35179=CARTESIAN_POINT('Origin',(54.9397894030341,37.9543320991532,22.6294657090004));
#35180=CARTESIAN_POINT('',(54.6185792877992,30.0858856793146,22.9294657090004));
#35181=CARTESIAN_POINT('Ctrl Pts',(54.4344015586084,29.7949688809415,22.6294657090004));
#35182=CARTESIAN_POINT('Ctrl Pts',(54.5282117103925,29.943146128711,22.783158980636));
#35183=CARTESIAN_POINT('Ctrl Pts',(54.6185792877992,30.0858856793146,22.9294657090004));
#35184=CARTESIAN_POINT('',(54.7784317609826,29.7809246878375,22.6294657090004));
#35185=CARTESIAN_POINT('Ctrl Pts',(54.6185792877992,30.0858856793146,22.9294657090004));
#35186=CARTESIAN_POINT('Ctrl Pts',(54.6970115760434,29.9362552863001,22.783158980636));
#35187=CARTESIAN_POINT('Ctrl Pts',(54.7784317609826,29.7809246878375,22.6294657090004));
#35188=CARTESIAN_POINT('',(55.1011470450858,29.7809246878375,22.6294657090004));
#35189=CARTESIAN_POINT('Origin',(54.9397894030341,37.9543320991532,22.6294657090004));
#35190=CARTESIAN_POINT('',(55.2609995182692,30.0858856793146,22.9294657090004));
#35191=CARTESIAN_POINT('Ctrl Pts',(55.1011470450858,29.7809246878374,22.6294657090004));
#35192=CARTESIAN_POINT('Ctrl Pts',(55.182567230025,29.9362552863001,22.783158980636));
#35193=CARTESIAN_POINT('Ctrl Pts',(55.2609995182692,30.0858856793146,22.9294657090004));
#35194=CARTESIAN_POINT('',(55.44517724746,29.7949688809415,22.6294657090004));
#35195=CARTESIAN_POINT('Ctrl Pts',(55.2609995182692,30.0858856793146,22.9294657090003));
#35196=CARTESIAN_POINT('Ctrl Pts',(55.3513670956759,29.943146128711,22.783158980636));
#35197=CARTESIAN_POINT('Ctrl Pts',(55.44517724746,29.7949688809415,22.6294657090004));
#35198=CARTESIAN_POINT('',(55.7668187230776,29.8212731725384,22.6294657090004));
#35199=CARTESIAN_POINT('Origin',(54.9397894030341,37.9543320991532,22.6294657090004));
#35200=CARTESIAN_POINT('',(55.9012821484182,30.1382488920364,22.9294657090004));
#35201=CARTESIAN_POINT('Ctrl Pts',(55.7668187230776,29.8212731725384,22.6294657090004));
#35202=CARTESIAN_POINT('Ctrl Pts',(55.8353071032744,29.9827234221893,22.783158980636));
#35203=CARTESIAN_POINT('Ctrl Pts',(55.9012821484182,30.1382488920364,22.9294657090004));
#35204=CARTESIAN_POINT('',(56.108559461216,29.8633122900625,22.6294657090004));
#35205=CARTESIAN_POINT('Ctrl Pts',(55.9012821484182,30.1382488920364,22.9294657090004));
#35206=CARTESIAN_POINT('Ctrl Pts',(56.0029836336695,30.0033500920025,22.7831589806361));
#35207=CARTESIAN_POINT('Ctrl Pts',(56.108559461216,29.8633122900626,22.6294657090004));
#35208=CARTESIAN_POINT('',(56.4269866573947,29.9157458225358,22.6294657090004));
#35209=CARTESIAN_POINT('Origin',(54.9397894030341,37.9543320991532,22.6294657090004));
#35210=CARTESIAN_POINT('',(56.5351662029818,30.2426268489385,22.9294657090004));
#35211=CARTESIAN_POINT('Ctrl Pts',(56.4269866573947,29.9157458225358,22.6294657090004));
#35212=CARTESIAN_POINT('Ctrl Pts',(56.4820874539788,30.0822412986007,22.783158980636));
#35213=CARTESIAN_POINT('Ctrl Pts',(56.5351662029818,30.2426268489385,22.9294657090004));
#35214=CARTESIAN_POINT('',(56.7641637030682,29.9855001010888,22.6294657090004));
#35215=CARTESIAN_POINT('Ctrl Pts',(56.5351662029818,30.2426268489385,22.9294657090004));
#35216=CARTESIAN_POINT('Ctrl Pts',(56.6475247894728,30.1164665287319,22.783158980636));
#35217=CARTESIAN_POINT('Ctrl Pts',(56.7641637030682,29.9855001010888,22.6294657090004));
#35218=CARTESIAN_POINT('',(57.0772575393543,30.0637139379306,22.6294657090004));
#35219=CARTESIAN_POINT('Origin',(54.9397894030341,37.9543320991532,22.6294657090004));
#35220=CARTESIAN_POINT('',(57.1584332881605,30.3983249319391,22.9294657090004));
#35221=CARTESIAN_POINT('Ctrl Pts',(57.0772575393543,30.0637139379306,22.6294657090004));
#35222=CARTESIAN_POINT('Ctrl Pts',(57.1186040656154,30.2341466404863,22.783158980636));
#35223=CARTESIAN_POINT('Ctrl Pts',(57.1584332881605,30.3983249319391,22.9294657090004));
#35224=CARTESIAN_POINT('',(57.4076270349543,30.1607191742974,22.6294657090004));
#35225=CARTESIAN_POINT('Ctrl Pts',(57.1584332881605,30.3983249319391,22.9294657090004));
#35226=CARTESIAN_POINT('Ctrl Pts',(57.2807012480359,30.2817426676757,22.783158980636));
#35227=CARTESIAN_POINT('Ctrl Pts',(57.4076270349542,30.1607191742974,22.6294657090004));
#35228=CARTESIAN_POINT('',(57.7133039235241,30.264192815328,22.6294657090004));
#35229=CARTESIAN_POINT('Origin',(54.9397894030341,37.9543320991532,22.6294657090004));
#35230=CARTESIAN_POINT('',(57.766935664334,30.604306995984,22.9294657090004));
#35231=CARTESIAN_POINT('Ctrl Pts',(57.7133039235241,30.264192815328,22.6294657090004));
#35232=CARTESIAN_POINT('Ctrl Pts',(57.7406210251516,30.4374285428584,22.783158980636));
#35233=CARTESIAN_POINT('Ctrl Pts',(57.766935664334,30.604306995984,22.9294657090003));
#35234=CARTESIAN_POINT('',(58.0346673145644,30.3878034556654,22.6294657090004));
#35235=CARTESIAN_POINT('Ctrl Pts',(57.766935664334,30.604306995984,22.9294657090004));
#35236=CARTESIAN_POINT('Ctrl Pts',(57.8982993244938,30.4980786233977,22.783158980636));
#35237=CARTESIAN_POINT('Ctrl Pts',(58.0346673145644,30.3878034556654,22.6294657090004));
#35238=CARTESIAN_POINT('',(58.3308930261577,30.5158483008756,22.6294657090004));
#35239=CARTESIAN_POINT('Origin',(54.9397894030341,37.9543320991532,22.6294657090004));
#35240=CARTESIAN_POINT('',(58.356623848585,30.8592022644217,22.9294657090004));
#35241=CARTESIAN_POINT('Ctrl Pts',(58.3308930261577,30.5158483008756,22.6294657090004));
#35242=CARTESIAN_POINT('Ctrl Pts',(58.3439989123473,30.6907341981958,22.783158980636));
#35243=CARTESIAN_POINT('Ctrl Pts',(58.356623848585,30.8592022644217,22.9294657090004));
#35244=CARTESIAN_POINT('',(58.6411116922923,30.6652417367664,22.6294657090004));
#35245=CARTESIAN_POINT('Ctrl Pts',(58.356623848585,30.8592022644217,22.9294657090004));
#35246=CARTESIAN_POINT('Ctrl Pts',(58.4962090055442,30.7640347158058,22.783158980636));
#35247=CARTESIAN_POINT('Ctrl Pts',(58.6411116922923,30.6652417367664,22.6294657090004));
#35248=CARTESIAN_POINT('',(58.9259148936722,30.8170056688373,22.6294657090004));
#35249=CARTESIAN_POINT('Origin',(54.9397894030341,37.9543320991532,22.6294657090004));
#35250=CARTESIAN_POINT('',(58.9235735633387,31.1613144512955,22.9294657090004));
#35251=CARTESIAN_POINT('Ctrl Pts',(58.9259148936722,30.8170056688373,22.6294657090004));
#35252=CARTESIAN_POINT('Ctrl Pts',(58.9247223469135,30.9923778991548,22.783158980636));
#35253=CARTESIAN_POINT('Ctrl Pts',(58.9235735633387,31.1613144512955,22.9294657090004));
#35254=CARTESIAN_POINT('',(59.2229243808604,30.9911877116138,22.6294657090004));
#35255=CARTESIAN_POINT('Ctrl Pts',(58.9235735633387,31.1613144512955,22.9294657090004));
#35256=CARTESIAN_POINT('Ctrl Pts',(59.0704513009078,31.0778410509844,22.783158980636));
#35257=CARTESIAN_POINT('Ctrl Pts',(59.2229243808603,30.9911877116138,22.6294657090004));
#35258=CARTESIAN_POINT('',(59.4944097537108,31.1656607666168,22.6294657090004));
#35259=CARTESIAN_POINT('Origin',(54.9397894030341,37.9543320991532,22.6294657090004));
#35260=CARTESIAN_POINT('',(59.4640118517838,31.5086330498468,22.9294657090004));
#35261=CARTESIAN_POINT('Ctrl Pts',(59.4944097537109,31.1656607666168,22.6294657090004));
#35262=CARTESIAN_POINT('Ctrl Pts',(59.478926710206,31.3403522566732,22.783158980636));
#35263=CARTESIAN_POINT('Ctrl Pts',(59.4640118517838,31.5086330498468,22.9294657090004));
#35264=CARTESIAN_POINT('',(59.7762335128185,31.3634722635224,22.6294657090004));
#35265=CARTESIAN_POINT('Ctrl Pts',(59.4640118517839,31.5086330498468,22.9294657090004));
#35266=CARTESIAN_POINT('Ctrl Pts',(59.6172047228522,31.4374092995474,22.783158980636));
#35267=CARTESIAN_POINT('Ctrl Pts',(59.7762335128185,31.3634722635223,22.6294657090004));
#35268=CARTESIAN_POINT('',(60.0325943667752,31.5594933520624,22.6294657090004));
#35269=CARTESIAN_POINT('Origin',(54.9397894030341,37.9543320991532,22.6294657090004));
#35270=CARTESIAN_POINT('',(59.9743421862767,31.8988467121058,22.9294657090004));
#35271=CARTESIAN_POINT('Ctrl Pts',(60.0325943667752,31.5594933520624,22.6294657090004));
#35272=CARTESIAN_POINT('Ctrl Pts',(60.0029238636241,31.7323415588135,22.783158980636));
#35273=CARTESIAN_POINT('Ctrl Pts',(59.9743421862767,31.8988467121058,22.9294657090004));
#35274=CARTESIAN_POINT('',(60.2973569071831,31.7796179002217,22.6294657090004));
#35275=CARTESIAN_POINT('Ctrl Pts',(59.9743421862767,31.8988467121058,22.9294657090004));
#35276=CARTESIAN_POINT('Ctrl Pts',(60.1328307175625,31.8403465941253,22.783158980636));
#35277=CARTESIAN_POINT('Ctrl Pts',(60.2973569071831,31.7796179002217,22.6294657090004));
#35278=CARTESIAN_POINT('',(60.5368872030596,31.9958825342957,22.6294657090004));
#35279=CARTESIAN_POINT('Origin',(54.9397894030341,37.9543320991532,22.6294657090004));
#35280=CARTESIAN_POINT('',(60.4511684026397,32.3293586305308,22.9294657090004));
#35281=CARTESIAN_POINT('Ctrl Pts',(60.5368872030596,31.9958825342957,22.6294657090004));
#35282=CARTESIAN_POINT('Ctrl Pts',(60.4932266925653,32.1657371814435,22.7831589806361));
#35283=CARTESIAN_POINT('Ctrl Pts',(60.4511684026397,32.3293586305308,22.9294657090004));
#35284=CARTESIAN_POINT('',(60.7828265737441,32.2368552411588,22.6294657090004));
#35285=CARTESIAN_POINT('Ctrl Pts',(60.4511684026397,32.3293586305308,22.9294657090004));
#35286=CARTESIAN_POINT('Ctrl Pts',(60.6138978791162,32.2839714535025,22.783158980636));
#35287=CARTESIAN_POINT('Ctrl Pts',(60.7828265737441,32.2368552411588,22.6294657090004));
#35288=CARTESIAN_POINT('',(61.0039322769409,32.4719242153082,22.6294657090004));
#35289=CARTESIAN_POINT('Origin',(54.9397894030341,37.9543320991532,22.6294657090004));
#35290=CARTESIAN_POINT('',(60.891317301074,32.7973038193341,22.9294657090004));
#35291=CARTESIAN_POINT('Ctrl Pts',(61.0039322769409,32.4719242153082,22.6294657090004));
#35292=CARTESIAN_POINT('Ctrl Pts',(60.9465723125975,32.6376549481999,22.783158980636));
#35293=CARTESIAN_POINT('Ctrl Pts',(60.891317301074,32.7973038193341,22.9294657090004));
#35294=CARTESIAN_POINT('',(61.2294117919672,32.7321414472685,22.6294657090004));
#35295=CARTESIAN_POINT('Ctrl Pts',(60.891317301074,32.7973038193341,22.9294657090004));
#35296=CARTESIAN_POINT('Ctrl Pts',(61.0572047849235,32.7653316274328,22.783158980636));
#35297=CARTESIAN_POINT('Ctrl Pts',(61.2294117919672,32.7321414472685,22.6294657090004));
#35298=CARTESIAN_POINT('',(61.4306214805095,32.9844504162541,22.6294657090004));
#35299=CARTESIAN_POINT('Origin',(54.9397894030341,37.9543320991532,22.6294657090004));
#35300=CARTESIAN_POINT('',(61.2918597632797,33.2995681804899,22.9294657090004));
#35301=CARTESIAN_POINT('Ctrl Pts',(61.4306214805095,32.9844504162541,22.6294657090004));
#35302=CARTESIAN_POINT('Ctrl Pts',(61.3599437834158,33.144954324206,22.783158980636));
#35303=CARTESIAN_POINT('Ctrl Pts',(61.2918597632797,33.2995681804899,22.9294657090004));
#35304=CARTESIAN_POINT('',(61.6341406109067,33.2621804705658,22.6294657090004));
#35305=CARTESIAN_POINT('Ctrl Pts',(61.2918597632797,33.2995681804899,22.9294657090004));
#35306=CARTESIAN_POINT('Ctrl Pts',(61.4598013006668,33.2812237433776,22.783158980636));
#35307=CARTESIAN_POINT('Ctrl Pts',(61.6341406109067,33.2621804705658,22.6294657090004));
#35308=CARTESIAN_POINT('',(61.8141152675145,33.5300503598269,22.6294657090004));
#35309=CARTESIAN_POINT('Origin',(54.9397894030341,37.9543320991532,22.6294657090004));
#35310=CARTESIAN_POINT('',(61.6501302452559,33.8328092275425,22.9294657090004));
#35311=CARTESIAN_POINT('Ctrl Pts',(61.8141152675145,33.5300503598269,22.6294657090004));
#35312=CARTESIAN_POINT('Ctrl Pts',(61.7305901860837,33.6842593158128,22.783158980636));
#35313=CARTESIAN_POINT('Ctrl Pts',(61.6501302452559,33.8328092275425,22.9294657090004));
#35314=CARTESIAN_POINT('',(61.9943196270479,33.8234449888007,22.6294657090004));
#35315=CARTESIAN_POINT('Ctrl Pts',(61.6501302452559,33.8328092275425,22.9294657090004));
#35316=CARTESIAN_POINT('Ctrl Pts',(61.8190082129576,33.8282146244215,22.783158980636));
#35317=CARTESIAN_POINT('Ctrl Pts',(61.9943196270479,33.8234449888007,22.6294657090004));
#35318=CARTESIAN_POINT('',(62.1518615500752,34.1050931684198,22.6294657090004));
#35319=CARTESIAN_POINT('Origin',(54.9397894030341,37.9543320991532,22.6294657090004));
#35320=CARTESIAN_POINT('',(61.9637445160554,34.3934783293021,22.9294657090004));
#35321=CARTESIAN_POINT('Ctrl Pts',(62.1518615500752,34.1050931684198,22.6294657090004));
#35322=CARTESIAN_POINT('Ctrl Pts',(62.0560449299436,34.2519809372804,22.783158980636));
#35323=CARTESIAN_POINT('Ctrl Pts',(61.9637445160554,34.3934783293021,22.9294657090004));
#35324=CARTESIAN_POINT('',(62.3075519084639,34.4121998792067,22.6294657090004));
#35325=CARTESIAN_POINT('Ctrl Pts',(61.9637445160554,34.3934783293021,22.9294657090004));
#35326=CARTESIAN_POINT('Ctrl Pts',(62.1324350590596,34.4026641364983,22.783158980636));
#35327=CARTESIAN_POINT('Ctrl Pts',(62.3075519084639,34.4121998792067,22.6294657090004));
#35328=CARTESIAN_POINT('',(62.4416126824056,34.705752027017,22.6294657090004));
#35329=CARTESIAN_POINT('Origin',(54.9397894030341,37.9543320991532,22.6294657090004));
#35330=CARTESIAN_POINT('',(62.2306155244487,34.9778443254007,22.9294657090004));
#35331=CARTESIAN_POINT('Ctrl Pts',(62.4416126824056,34.705752027017,22.6294657090004));
#35332=CARTESIAN_POINT('Ctrl Pts',(62.3341421673715,34.8443410948853,22.783158980636));
#35333=CARTESIAN_POINT('Ctrl Pts',(62.2306155244488,34.9778443254007,22.9294657090004));
#35334=CARTESIAN_POINT('',(62.5717529460015,35.0245270751257,22.6294657090004));
#35335=CARTESIAN_POINT('Ctrl Pts',(62.2306155244487,34.9778443254006,22.9294657090003));
#35336=CARTESIAN_POINT('Ctrl Pts',(62.3979960350237,35.0007494128826,22.783158980636));
#35337=CARTESIAN_POINT('Ctrl Pts',(62.5717529460015,35.0245270751257,22.6294657090004));
#35338=CARTESIAN_POINT('',(62.6814404185254,35.3280296500162,22.6294657090004));
#35339=CARTESIAN_POINT('Origin',(54.9397894030341,37.9543320991532,22.6294657090004));
#35340=CARTESIAN_POINT('',(62.4489672879057,35.5820183565476,22.9294657090004));
#35341=CARTESIAN_POINT('Ctrl Pts',(62.6814404185254,35.3280296500163,22.6294657090004));
#35342=CARTESIAN_POINT('Ctrl Pts',(62.563031207135,35.4573977295112,22.783158980636));
#35343=CARTESIAN_POINT('Ctrl Pts',(62.4489672879057,35.5820183565476,22.9294657090003));
#35344=CARTESIAN_POINT('',(62.785164525346,35.6563516400959,22.6294657090004));
#35345=CARTESIAN_POINT('Ctrl Pts',(62.4489672879057,35.5820183565476,22.9294657090004));
#35346=CARTESIAN_POINT('Ctrl Pts',(62.6139238763694,35.6184902947372,22.783158980636));
#35347=CARTESIAN_POINT('Ctrl Pts',(62.785164525346,35.6563516400959,22.6294657090004));
#35348=CARTESIAN_POINT('',(62.8697487444197,35.9677848825051,22.6294657090004));
#35349=CARTESIAN_POINT('Origin',(54.9397894030341,37.9543320991532,22.6294657090004));
#35350=CARTESIAN_POINT('',(62.617346711466,36.2019797442473,22.9294657090004));
#35351=CARTESIAN_POINT('Ctrl Pts',(62.8697487444197,35.9677848825051,22.6294657090004));
#35352=CARTESIAN_POINT('Ctrl Pts',(62.7411888304386,36.0870710504019,22.783158980636));
#35353=CARTESIAN_POINT('Ctrl Pts',(62.617346711466,36.2019797442473,22.9294657090004));
#35354=CARTESIAN_POINT('',(62.9463664276474,36.3034688858809,22.6294657090003));
#35355=CARTESIAN_POINT('Ctrl Pts',(62.617346711466,36.2019797442473,22.9294657090004));
#35356=CARTESIAN_POINT('Ctrl Pts',(62.7787816189382,36.2517758184133,22.783158980636));
#35357=CARTESIAN_POINT('Ctrl Pts',(62.9463664276474,36.3034688858809,22.6294657090004));
#35358=CARTESIAN_POINT('',(63.0052844992482,36.6207602589636,22.6294657090003));
#35359=CARTESIAN_POINT('Origin',(54.9397894030341,37.9543320991532,22.6294657090004));
#35360=CARTESIAN_POINT('',(62.7346332578465,36.8336027477512,22.9294657090004));
#35361=CARTESIAN_POINT('Ctrl Pts',(63.0052844992482,36.6207602589636,22.6294657090004));
#35362=CARTESIAN_POINT('Ctrl Pts',(62.8674294276931,36.7291706854956,22.783158980636));
#35363=CARTESIAN_POINT('Ctrl Pts',(62.7346332578465,36.8336027477512,22.9294657090004));
#35364=CARTESIAN_POINT('',(63.0542858808421,36.9615723539771,22.6294657090003));
#35365=CARTESIAN_POINT('Ctrl Pts',(62.7346332578465,36.8336027477512,22.9294657090004));
#35366=CARTESIAN_POINT('Ctrl Pts',(62.8914721616528,36.8963915732358,22.783158980636));
#35367=CARTESIAN_POINT('Ctrl Pts',(63.0542858808421,36.9615723539771,22.6294657090004));
#35368=CARTESIAN_POINT('',(63.0871457149245,37.2826103359947,22.6294657090003));
#35369=CARTESIAN_POINT('Origin',(54.9397894030341,37.9543320991532,22.6294657090004));
#35370=CARTESIAN_POINT('',(62.8000464044319,37.4726840201813,22.9294657090004));
#35371=CARTESIAN_POINT('Ctrl Pts',(63.0871457149245,37.2826103359947,22.6294657090004));
#35372=CARTESIAN_POINT('Ctrl Pts',(62.9409128885521,37.3794235676598,22.783158980636));
#35373=CARTESIAN_POINT('Ctrl Pts',(62.8000464044319,37.4726840201813,22.9294657090004));
#35374=CARTESIAN_POINT('',(63.1082046987747,37.6262824743835,22.6294657090003));
#35375=CARTESIAN_POINT('Ctrl Pts',(62.8000464044319,37.4726840201813,22.9294657090004));
#35376=CARTESIAN_POINT('Ctrl Pts',(62.951245567544,37.5480477477104,22.783158980636));
#35377=CARTESIAN_POINT('Ctrl Pts',(63.1082046987747,37.6262824743835,22.6294657090004));
#35378=CARTESIAN_POINT('',(63.1147876185643,37.9489306105332,22.6294657090003));
#35379=CARTESIAN_POINT('Origin',(54.9397894030341,37.9543320991532,22.6294657090004));
#35380=CARTESIAN_POINT('',(63.1049749955285,37.9543320991532,22.639280116506));
#35381=CARTESIAN_POINT('Ctrl Pts',(63.1147876185642,37.9489306105333,22.6294657090004));
#35382=CARTESIAN_POINT('Ctrl Pts',(63.1098783601679,37.9516329769916,22.6343767518666));
#35383=CARTESIAN_POINT('Ctrl Pts',(63.1049749955285,37.9543320991532,22.639280116506));
#35384=CARTESIAN_POINT('',(62.7147894030341,37.9543320991532,23.0294657090004));
#35385=CARTESIAN_POINT('',(63.1147894030342,37.9543320991532,22.6294657090004));
#35386=CARTESIAN_POINT('Origin',(54.9397894030341,37.9543320991532,23.0294657090004));
#35387=CARTESIAN_POINT('',(62.8131508375241,38.1149705811106,22.9294657090004));
#35388=CARTESIAN_POINT('Ctrl Pts',(63.1049749955285,37.9543320991532,22.639280116506));
#35389=CARTESIAN_POINT('Ctrl Pts',(62.9564231974998,38.0361044085143,22.7878319145347));
#35390=CARTESIAN_POINT('Ctrl Pts',(62.8131508375241,38.1149705811106,22.9294657090004));
#35391=CARTESIAN_POINT('',(63.1077640606078,38.2931757109184,22.6294657090003));
#35392=CARTESIAN_POINT('Ctrl Pts',(62.8131508375241,38.1149705811106,22.9294657090004));
#35393=CARTESIAN_POINT('Ctrl Pts',(62.9577040544577,38.2024076775117,22.783158980636));
#35394=CARTESIAN_POINT('Ctrl Pts',(63.1077640606078,38.2931757109184,22.6294657090004));
#35395=CARTESIAN_POINT('',(63.0880262578595,38.6152868310874,22.6294657090003));
#35396=CARTESIAN_POINT('Origin',(54.9397894030341,37.9543320991532,22.6294657090004));
#35397=CARTESIAN_POINT('',(62.773859349283,38.756188119446,22.9294657090004));
#35398=CARTESIAN_POINT('Ctrl Pts',(63.0880262578595,38.6152868310874,22.6294657090004));
#35399=CARTESIAN_POINT('Ctrl Pts',(62.9280066642388,38.6870543097374,22.783158980636));
#35400=CARTESIAN_POINT('Ctrl Pts',(62.7738593492831,38.756188119446,22.9294657090004));
#35401=CARTESIAN_POINT('',(63.0529668987158,38.9578139991223,22.6294657090003));
#35402=CARTESIAN_POINT('Ctrl Pts',(62.7738593492831,38.756188119446,22.9294657090004));
#35403=CARTESIAN_POINT('Ctrl Pts',(62.910804642229,38.8551167052685,22.783158980636));
#35404=CARTESIAN_POINT('Ctrl Pts',(63.0529668987157,38.9578139991223,22.6294657090004));
#35405=CARTESIAN_POINT('',(63.0070397252503,39.2772445069504,22.6294657090003));
#35406=CARTESIAN_POINT('Origin',(54.9397894030341,37.9543320991532,22.6294657090004));
#35407=CARTESIAN_POINT('',(62.6824334180802,39.3920694382633,22.9294657090004));
#35408=CARTESIAN_POINT('Ctrl Pts',(63.0070397252503,39.2772445069504,22.6294657090004));
#35409=CARTESIAN_POINT('Ctrl Pts',(62.8417028678599,39.335730102806,22.7831589806361));
#35410=CARTESIAN_POINT('Ctrl Pts',(62.6824334180802,39.3920694382633,22.9294657090004));
#35411=CARTESIAN_POINT('',(62.94417787917,39.6157742808448,22.6294657090003));
#35412=CARTESIAN_POINT('Ctrl Pts',(62.6824334180802,39.3920694382633,22.9294657090004));
#35413=CARTESIAN_POINT('Ctrl Pts',(62.8108594387084,39.5018311600907,22.7831589806361));
#35414=CARTESIAN_POINT('Ctrl Pts',(62.94417787917,39.6157742808448,22.6294657090004));
#35415=CARTESIAN_POINT('',(62.8723669727493,39.9303984190047,22.6294657090004));
#35416=CARTESIAN_POINT('Origin',(54.9397894030341,37.9543320991532,22.6294657090004));
#35417=CARTESIAN_POINT('',(62.5394814684036,40.0183828522987,22.9294657090004));
#35418=CARTESIAN_POINT('Ctrl Pts',(62.8723669727493,39.9303984190047,22.6294657090004));
#35419=CARTESIAN_POINT('Ctrl Pts',(62.7028131410966,39.975212920075,22.783158980636));
#35420=CARTESIAN_POINT('Ctrl Pts',(62.5394814684036,40.0183828522987,22.9294657090004));
#35421=CARTESIAN_POINT('',(62.7821209749467,40.2626779389667,22.6294657090004));
#35422=CARTESIAN_POINT('Ctrl Pts',(62.5394814684036,40.0183828522987,22.9294657090004));
#35423=CARTESIAN_POINT('Ctrl Pts',(62.6585335627355,40.1382472639816,22.783158980636));
#35424=CARTESIAN_POINT('Ctrl Pts',(62.7821209749467,40.2626779389667,22.6294657090003));
#35425=CARTESIAN_POINT('',(62.6849042253051,40.5704019357284,22.6294657090004));
#35426=CARTESIAN_POINT('Origin',(54.9397894030341,37.9543320991532,22.6294657090004));
#35427=CARTESIAN_POINT('',(62.3459548218929,40.6309603491164,22.9294657090004));
#35428=CARTESIAN_POINT('Ctrl Pts',(62.6849042253051,40.5704019357284,22.6294657090004));
#35429=CARTESIAN_POINT('Ctrl Pts',(62.5122617721653,40.6012471089027,22.783158980636));
#35430=CARTESIAN_POINT('Ctrl Pts',(62.3459548218929,40.6309603491164,22.9294657090004));
#35431=CARTESIAN_POINT('',(62.5678746480059,40.894219936375,22.6294657090004));
#35432=CARTESIAN_POINT('Ctrl Pts',(62.3459548218929,40.6309603491164,22.9294657090004));
#35433=CARTESIAN_POINT('Ctrl Pts',(62.4548407178829,40.7601297727713,22.783158980636));
#35434=CARTESIAN_POINT('Ctrl Pts',(62.5678746480059,40.894219936375,22.6294657090004));
#35435=CARTESIAN_POINT('',(62.4458990165727,41.1929959393108,22.6294657090004));
#35436=CARTESIAN_POINT('Origin',(54.9397894030341,37.9543320991532,22.6294657090004));
#35437=CARTESIAN_POINT('',(62.1031413664509,41.2257253265432,22.9294657090004));
#35438=CARTESIAN_POINT('Ctrl Pts',(62.4458990165727,41.1929959393108,22.6294657090004));
#35439=CARTESIAN_POINT('Ctrl Pts',(62.2713168489873,41.2096665150507,22.783158980636));
#35440=CARTESIAN_POINT('Ctrl Pts',(62.1031413664509,41.2257253265432,22.9294657090004));
#35441=CARTESIAN_POINT('',(62.3028646723053,41.5061974652739,22.6294657090004));
#35442=CARTESIAN_POINT('Ctrl Pts',(62.1031413664509,41.2257253265432,22.9294657090004));
#35443=CARTESIAN_POINT('Ctrl Pts',(62.2011364464262,41.3633401609671,22.783158980636));
#35444=CARTESIAN_POINT('Ctrl Pts',(62.3028646723053,41.5061974652739,22.6294657090004));
#35445=CARTESIAN_POINT('',(62.1569418867831,41.7940371693789,22.6294657090004));
#35446=CARTESIAN_POINT('Origin',(54.9397894030341,37.9543320991532,22.6294657090004));
#35447=CARTESIAN_POINT('',(61.8126569855623,41.7987197217835,22.9294657090004));
#35448=CARTESIAN_POINT('Ctrl Pts',(62.156941886783,41.7940371693789,22.6294657090004));
#35449=CARTESIAN_POINT('Ctrl Pts',(61.9815818202734,41.7964222077532,22.783158980636));
#35450=CARTESIAN_POINT('Ctrl Pts',(61.8126569855623,41.7987197217835,22.9294657090004));
#35451=CARTESIAN_POINT('',(61.9888546455096,42.0945379161778,22.6294657090004));
#35452=CARTESIAN_POINT('Ctrl Pts',(61.8126569855623,41.7987197217835,22.9294657090004));
#35453=CARTESIAN_POINT('Ctrl Pts',(61.8991091084337,41.9438641629583,22.783158980636));
#35454=CARTESIAN_POINT('Ctrl Pts',(61.9888546455096,42.0945379161778,22.6294657090004));
#35455=CARTESIAN_POINT('',(61.8199557979604,42.3695257957114,22.6294657090004));
#35456=CARTESIAN_POINT('Origin',(54.9397894030341,37.9543320991532,22.6294657090004));
#35457=CARTESIAN_POINT('',(61.4764348048553,42.3461303516746,22.9294657090004));
#35458=CARTESIAN_POINT('Ctrl Pts',(61.8199557979604,42.3695257957114,22.6294657090004));
#35459=CARTESIAN_POINT('Ctrl Pts',(61.6449848248368,42.3576094246833,22.783158980636));
#35460=CARTESIAN_POINT('Ctrl Pts',(61.4764348048553,42.3461303516746,22.9294657090004));
#35461=CARTESIAN_POINT('',(61.6279342525392,42.6553259804552,22.6294657090004));
#35462=CARTESIAN_POINT('Ctrl Pts',(61.4764348048553,42.3461303516746,22.9294657090004));
#35463=CARTESIAN_POINT('Ctrl Pts',(61.5507686460086,42.4978384872913,22.783158980636));
#35464=CARTESIAN_POINT('Ctrl Pts',(61.6279342525392,42.6553259804552,22.6294657090004));
#35465=CARTESIAN_POINT('',(61.4371833369271,42.915632036449,22.6294657090004));
#35466=CARTESIAN_POINT('Origin',(54.9397894030341,37.9543320991532,22.6294657090004));
#35467=CARTESIAN_POINT('',(61.0967123274698,42.8643142887908,22.9294657090004));
#35468=CARTESIAN_POINT('Ctrl Pts',(61.4371833369271,42.915632036449,22.6294657090004));
#35469=CARTESIAN_POINT('Ctrl Pts',(61.2637658601475,42.8894935575016,22.783158980636));
#35470=CARTESIAN_POINT('Ctrl Pts',(61.0967123274698,42.8643142887908,22.9294657090004));
#35471=CARTESIAN_POINT('',(61.2225053590615,43.184829706062,22.6294657090004));
#35472=CARTESIAN_POINT('Ctrl Pts',(61.0967123274698,42.8643142887908,22.9294657090004));
#35473=CARTESIAN_POINT('Ctrl Pts',(61.1584332074564,43.021576526237,22.783158980636));
#35474=CARTESIAN_POINT('Ctrl Pts',(61.2225053590615,43.184829706062,22.6294657090004));
#35475=CARTESIAN_POINT('',(61.0111717912583,43.4287216446607,22.6294657090004));
#35476=CARTESIAN_POINT('Origin',(54.9397894030341,37.9543320991532,22.6294657090004));
#35477=CARTESIAN_POINT('',(60.6760165438429,43.3498231045251,22.9294657090004));
#35478=CARTESIAN_POINT('Ctrl Pts',(61.0111717912583,43.4287216446607,22.6294657090004));
#35479=CARTESIAN_POINT('Ctrl Pts',(60.8404618755187,43.3885350050589,22.783158980636));
#35480=CARTESIAN_POINT('Ctrl Pts',(60.6760165438429,43.3498231045251,22.9294657090004));
#35481=CARTESIAN_POINT('',(60.7752660274717,43.6795253330662,22.6294657090004));
#35482=CARTESIAN_POINT('Ctrl Pts',(60.6760165438429,43.3498231045251,22.9294657090004));
#35483=CARTESIAN_POINT('Ctrl Pts',(60.7247137203897,43.5115928895569,22.783158980636));
#35484=CARTESIAN_POINT('Ctrl Pts',(60.7752660274716,43.6795253330662,22.6294657090004));
#35485=CARTESIAN_POINT('',(60.5447561975034,43.9053800936578,22.6294657090004));
#35486=CARTESIAN_POINT('Origin',(54.9397894030341,37.9543320991532,22.6294657090004));
#35487=CARTESIAN_POINT('',(60.2171471150049,43.7994258178119,22.9294657090004));
#35488=CARTESIAN_POINT('Ctrl Pts',(60.5447561975034,43.9053800936578,22.6294657090004));
#35489=CARTESIAN_POINT('Ctrl Pts',(60.377889889128,43.8514127288578,22.783158980636));
#35490=CARTESIAN_POINT('Ctrl Pts',(60.2171471150049,43.7994258178119,22.9294657090004));
#35491=CARTESIAN_POINT('',(60.289192561732,44.1361207436891,22.6294657090004));
#35492=CARTESIAN_POINT('Ctrl Pts',(60.2171471150049,43.7994258178119,22.9294657090004));
#35493=CARTESIAN_POINT('Ctrl Pts',(60.2524965164364,43.9646265992003,22.783158980636));
#35494=CARTESIAN_POINT('Ctrl Pts',(60.2891925617321,44.1361207436891,22.6294657090004));
#35495=CARTESIAN_POINT('',(60.0410404744858,44.3424353001052,22.6294657090004));
#35496=CARTESIAN_POINT('Origin',(54.9397894030341,37.9543320991532,22.6294657090004));
#35497=CARTESIAN_POINT('',(59.7231577412963,44.2101303967737,22.9294657090004));
#35498=CARTESIAN_POINT('Ctrl Pts',(60.0410404744858,44.3424353001052,22.6294657090004));
#35499=CARTESIAN_POINT('Ctrl Pts',(59.8791282412257,44.2750463540158,22.783158980636));
#35500=CARTESIAN_POINT('Ctrl Pts',(59.7231577412963,44.2101303967737,22.9294657090004));
#35501=CARTESIAN_POINT('',(59.7675197005607,44.551577370806,22.6294657090004));
#35502=CARTESIAN_POINT('Ctrl Pts',(59.7231577412963,44.2101303967737,22.9294657090004));
#35503=CARTESIAN_POINT('Ctrl Pts',(59.7449241231784,44.3776627905746,22.783158980636));
#35504=CARTESIAN_POINT('Ctrl Pts',(59.7675197005607,44.551577370806,22.6294657090004));
#35505=CARTESIAN_POINT('',(59.5033767672348,44.7369787337132,22.6294657090004));
#35506=CARTESIAN_POINT('Origin',(54.9397894030341,37.9543320991532,22.6294657090004));
#35507=CARTESIAN_POINT('',(59.1973358404969,44.5792036701988,22.9294657090004));
#35508=CARTESIAN_POINT('Ctrl Pts',(59.5033767672348,44.7369787337132,22.6294657090004));
#35509=CARTESIAN_POINT('Ctrl Pts',(59.3474961082889,44.6566166686521,22.7831589806361));
#35510=CARTESIAN_POINT('Ctrl Pts',(59.1973358404969,44.5792036701988,22.9294657090004));
#35511=CARTESIAN_POINT('',(59.2137190907787,44.9231304191088,22.6294657090004));
#35512=CARTESIAN_POINT('Ctrl Pts',(59.1973358404969,44.5792036701988,22.9294657090004));
#35513=CARTESIAN_POINT('Ctrl Pts',(59.2053743511492,44.7479527759724,22.783158980636));
#35514=CARTESIAN_POINT('Ctrl Pts',(59.2137190907787,44.9231304191088,22.6294657090004));
#35515=CARTESIAN_POINT('',(58.935343139014,45.0863847730261,22.6294657090004));
#35516=CARTESIAN_POINT('Origin',(54.9397894030341,37.9543320991532,22.6294657090004));
#35517=CARTESIAN_POINT('',(58.6431806706019,44.9041895163456,22.9294657090004));
#35518=CARTESIAN_POINT('Ctrl Pts',(58.935343139014,45.0863847730261,22.6294657090004));
#35519=CARTESIAN_POINT('Ctrl Pts',(58.7865314144489,44.9935843852776,22.783158980636));
#35520=CARTESIAN_POINT('Ctrl Pts',(58.6431806706019,44.9041895163456,22.9294657090004));
#35521=CARTESIAN_POINT('',(58.6314761840735,45.2483072643631,22.6294657090004));
#35522=CARTESIAN_POINT('Ctrl Pts',(58.6431806706019,44.9041895163456,22.9294657090004));
#35523=CARTESIAN_POINT('Ctrl Pts',(58.6374378150623,45.0730323366345,22.783158980636));
#35524=CARTESIAN_POINT('Ctrl Pts',(58.6314761840736,45.2483072643631,22.6294657090004));
#35525=CARTESIAN_POINT('',(58.3407197599002,45.3883281785002,22.6294657090004));
#35526=CARTESIAN_POINT('Origin',(54.9397894030341,37.9543320991532,22.6294657090004));
#35527=CARTESIAN_POINT('',(58.0643800428377,45.1829252080266,22.9294657090004));
#35528=CARTESIAN_POINT('Ctrl Pts',(58.3407197599002,45.3883281785002,22.6294657090004));
#35529=CARTESIAN_POINT('Ctrl Pts',(58.1999672871908,45.2837070393338,22.7831589806361));
#35530=CARTESIAN_POINT('Ctrl Pts',(58.0643800428377,45.1829252080266,22.9294657090004));
#35531=CARTESIAN_POINT('',(58.024665710926,45.5249439083142,22.6294657090004));
#35532=CARTESIAN_POINT('Ctrl Pts',(58.0643800428377,45.1829252080266,22.9294657090004));
#35533=CARTESIAN_POINT('Ctrl Pts',(58.0448940388624,45.3507381217191,22.783158980636));
#35534=CARTESIAN_POINT('Ctrl Pts',(58.024665710926,45.5249439083142,22.6294657090004));
#35535=CARTESIAN_POINT('',(57.7234637503755,45.6407995665893,22.6294657090004));
#35536=CARTESIAN_POINT('Origin',(54.9397894030341,37.9543320991532,22.6294657090004));
#35537=CARTESIAN_POINT('',(57.4647857798868,45.413555805202,22.9294657090004));
#35538=CARTESIAN_POINT('Ctrl Pts',(57.7234637503755,45.6407995665893,22.6294657090004));
#35539=CARTESIAN_POINT('Ctrl Pts',(57.5917072140051,45.5250539124248,22.783158980636));
#35540=CARTESIAN_POINT('Ctrl Pts',(57.4647857798868,45.4135558052021,22.9294657090004));
#35541=CARTESIAN_POINT('',(57.3973258949183,45.7511993797383,22.6294657090004));
#35542=CARTESIAN_POINT('Ctrl Pts',(57.4647857798868,45.413555805202,22.9294657090003));
#35543=CARTESIAN_POINT('Ctrl Pts',(57.4316863036172,45.5792220450446,22.783158980636));
#35544=CARTESIAN_POINT('Ctrl Pts',(57.3973258949183,45.7511993797383,22.6294657090004));
#35545=CARTESIAN_POINT('',(57.0876828473432,45.8421187818605,22.6294657090004));
#35546=CARTESIAN_POINT('Origin',(54.9397894030341,37.9543320991532,22.6294657090004));
#35547=CARTESIAN_POINT('',(56.8483880826431,45.594546499299,22.9294657090004));
#35548=CARTESIAN_POINT('Ctrl Pts',(57.0876828473432,45.8421187818605,22.6294657090004));
#35549=CARTESIAN_POINT('Ctrl Pts',(56.9657990653231,45.7160188809296,22.783158980636));
#35550=CARTESIAN_POINT('Ctrl Pts',(56.8483880826431,45.594546499299,22.9294657090004));
#35551=CARTESIAN_POINT('',(56.753631579022,45.9255679858027,22.6294657090004));
#35552=CARTESIAN_POINT('Ctrl Pts',(56.8483880826431,45.594546499299,22.9294657090004));
#35553=CARTESIAN_POINT('Ctrl Pts',(56.8018954056327,45.7569635837985,22.783158980636));
#35554=CARTESIAN_POINT('Ctrl Pts',(56.753631579022,45.9255679858026,22.6294657090004));
#35555=CARTESIAN_POINT('',(56.4376080678164,45.9909460781515,22.6294657090004));
#35556=CARTESIAN_POINT('Origin',(54.9397894030341,37.9543320991532,22.6294657090004));
#35557=CARTESIAN_POINT('',(56.2192889760832,45.7246928271096,22.9294657090004));
#35558=CARTESIAN_POINT('Ctrl Pts',(56.4376080678164,45.9909460781514,22.6294657090004));
#35559=CARTESIAN_POINT('Ctrl Pts',(56.3264081566065,45.85533110449,22.783158980636));
#35560=CARTESIAN_POINT('Ctrl Pts',(56.2192889760832,45.7246928271096,22.9294657090003));
#35561=CARTESIAN_POINT('',(56.0978664427074,46.0468893322027,22.6294657090004));
#35562=CARTESIAN_POINT('Ctrl Pts',(56.2192889760832,45.7246928271096,22.9294657090004));
#35563=CARTESIAN_POINT('Ctrl Pts',(56.1597124994268,45.8827798973656,22.783158980636));
#35564=CARTESIAN_POINT('Ctrl Pts',(56.0978664427074,46.0468893322027,22.6294657090004));
#35565=CARTESIAN_POINT('',(55.7775655521983,46.0862910343602,22.6294657090004));
#35566=CARTESIAN_POINT('Origin',(54.9397894030341,37.9543320991532,22.6294657090004));
#35567=CARTESIAN_POINT('',(55.5816750109672,45.803128686295,22.9294657090004));
#35568=CARTESIAN_POINT('Ctrl Pts',(55.7775655521982,46.0862910343601,22.6294657090004));
#35569=CARTESIAN_POINT('Ctrl Pts',(55.6777895288609,45.9420634832429,22.783158980636));
#35570=CARTESIAN_POINT('Ctrl Pts',(55.5816750109672,45.803128686295,22.9294657090003));
#35571=CARTESIAN_POINT('',(55.434394494763,46.1143560453948,22.6294657090004));
#35572=CARTESIAN_POINT('Ctrl Pts',(55.5816750109672,45.803128686295,22.9294657090003));
#35573=CARTESIAN_POINT('Ctrl Pts',(55.5094112062876,45.9558336989374,22.783158980636));
#35574=CARTESIAN_POINT('Ctrl Pts',(55.434394494763,46.1143560453948,22.6294657090004));
#35575=CARTESIAN_POINT('',(55.1119477745308,46.1275191455338,22.6294657090004));
#35576=CARTESIAN_POINT('Origin',(54.9397894030341,37.9543320991532,22.6294657090004));
#35577=CARTESIAN_POINT('',(54.9397894030341,45.8293320991532,22.9294657090004));
#35578=CARTESIAN_POINT('Ctrl Pts',(55.1119477745308,46.1275191455338,22.6294657090004));
#35579=CARTESIAN_POINT('Ctrl Pts',(55.0242596320395,45.9756388275175,22.783158980636));
#35580=CARTESIAN_POINT('Ctrl Pts',(54.9397894030341,45.8293320991532,22.9294657090004));
#35581=CARTESIAN_POINT('',(54.7676310315374,46.1275191455338,22.6294657090004));
#35582=CARTESIAN_POINT('Ctrl Pts',(54.9397894030341,45.8293320991532,22.9294657090004));
#35583=CARTESIAN_POINT('Ctrl Pts',(54.8553191740288,45.9756388275175,22.7831589806361));
#35584=CARTESIAN_POINT('Ctrl Pts',(54.7676310315374,46.1275191455338,22.6294657090004));
#35585=CARTESIAN_POINT('',(54.4451843113051,46.1143560453948,22.6294657090004));
#35586=CARTESIAN_POINT('Origin',(54.9397894030341,37.9543320991532,22.6294657090004));
#35587=CARTESIAN_POINT('',(54.297903795101,45.803128686295,22.9294657090004));
#35588=CARTESIAN_POINT('Ctrl Pts',(54.4451843113051,46.1143560453948,22.6294657090004));
#35589=CARTESIAN_POINT('Ctrl Pts',(54.3701675997806,45.9558336989374,22.783158980636));
#35590=CARTESIAN_POINT('Ctrl Pts',(54.297903795101,45.803128686295,22.9294657090004));
#35591=CARTESIAN_POINT('',(54.1020132538699,46.0862910343601,22.6294657090004));
#35592=CARTESIAN_POINT('Ctrl Pts',(54.297903795101,45.803128686295,22.9294657090004));
#35593=CARTESIAN_POINT('Ctrl Pts',(54.2017892772072,45.9420634832428,22.783158980636));
#35594=CARTESIAN_POINT('Ctrl Pts',(54.1020132538699,46.0862910343601,22.6294657090004));
#35595=CARTESIAN_POINT('',(53.7817123633608,46.0468893322027,22.6294657090004));
#35596=CARTESIAN_POINT('Origin',(54.9397894030341,37.9543320991532,22.6294657090004));
#35597=CARTESIAN_POINT('',(53.660289829985,45.7246928271096,22.9294657090004));
#35598=CARTESIAN_POINT('Ctrl Pts',(53.7817123633608,46.0468893322027,22.6294657090004));
#35599=CARTESIAN_POINT('Ctrl Pts',(53.7198663066414,45.8827798973656,22.7831589806361));
#35600=CARTESIAN_POINT('Ctrl Pts',(53.660289829985,45.7246928271096,22.9294657090004));
#35601=CARTESIAN_POINT('',(53.4419707382517,45.9909460781514,22.6294657090004));
#35602=CARTESIAN_POINT('Ctrl Pts',(53.660289829985,45.7246928271096,22.9294657090004));
#35603=CARTESIAN_POINT('Ctrl Pts',(53.5531706494617,45.8553311044899,22.783158980636));
#35604=CARTESIAN_POINT('Ctrl Pts',(53.4419707382517,45.9909460781514,22.6294657090004));
#35605=CARTESIAN_POINT('',(53.1259472270462,45.9255679858026,22.6294657090004));
#35606=CARTESIAN_POINT('Origin',(54.9397894030341,37.9543320991532,22.6294657090004));
#35607=CARTESIAN_POINT('',(53.0311907234251,45.594546499299,22.9294657090004));
#35608=CARTESIAN_POINT('Ctrl Pts',(53.1259472270462,45.9255679858026,22.6294657090004));
#35609=CARTESIAN_POINT('Ctrl Pts',(53.0776834004354,45.7569635837984,22.783158980636));
#35610=CARTESIAN_POINT('Ctrl Pts',(53.0311907234251,45.594546499299,22.9294657090004));
#35611=CARTESIAN_POINT('',(52.791895958725,45.8421187818605,22.6294657090004));
#35612=CARTESIAN_POINT('Ctrl Pts',(53.0311907234251,45.594546499299,22.9294657090004));
#35613=CARTESIAN_POINT('Ctrl Pts',(52.9137797407451,45.7160188809296,22.783158980636));
#35614=CARTESIAN_POINT('Ctrl Pts',(52.791895958725,45.8421187818605,22.6294657090004));
#35615=CARTESIAN_POINT('',(52.4822529111499,45.7511993797382,22.6294657090004));
#35616=CARTESIAN_POINT('Origin',(54.9397894030341,37.9543320991532,22.6294657090004));
#35617=CARTESIAN_POINT('',(52.4147930261813,45.413555805202,22.9294657090004));
#35618=CARTESIAN_POINT('Ctrl Pts',(52.4822529111499,45.7511993797382,22.6294657090004));
#35619=CARTESIAN_POINT('Ctrl Pts',(52.447892502451,45.5792220450445,22.783158980636));
#35620=CARTESIAN_POINT('Ctrl Pts',(52.4147930261813,45.413555805202,22.9294657090004));
#35621=CARTESIAN_POINT('',(52.1561150556927,45.6407995665893,22.6294657090004));
#35622=CARTESIAN_POINT('Ctrl Pts',(52.4147930261813,45.413555805202,22.9294657090004));
#35623=CARTESIAN_POINT('Ctrl Pts',(52.2878715920631,45.5250539124247,22.783158980636));
#35624=CARTESIAN_POINT('Ctrl Pts',(52.1561150556927,45.6407995665893,22.6294657090004));
#35625=CARTESIAN_POINT('',(51.8549130951421,45.5249439083141,22.6294657090004));
#35626=CARTESIAN_POINT('Origin',(54.9397894030341,37.9543320991532,22.6294657090004));
#35627=CARTESIAN_POINT('',(51.8151987632305,45.1829252080266,22.9294657090004));
#35628=CARTESIAN_POINT('Ctrl Pts',(51.8549130951421,45.5249439083141,22.6294657090004));
#35629=CARTESIAN_POINT('Ctrl Pts',(51.8346847672058,45.3507381217191,22.783158980636));
#35630=CARTESIAN_POINT('Ctrl Pts',(51.8151987632305,45.1829252080266,22.9294657090004));
#35631=CARTESIAN_POINT('',(51.5388590461679,45.3883281785002,22.6294657090004));
#35632=CARTESIAN_POINT('Ctrl Pts',(51.8151987632305,45.1829252080266,22.9294657090004));
#35633=CARTESIAN_POINT('Ctrl Pts',(51.6796115188774,45.2837070393337,22.783158980636));
#35634=CARTESIAN_POINT('Ctrl Pts',(51.5388590461679,45.3883281785002,22.6294657090004));
#35635=CARTESIAN_POINT('',(51.2481026219946,45.2483072643631,22.6294657090004));
#35636=CARTESIAN_POINT('Origin',(54.9397894030341,37.9543320991532,22.6294657090004));
#35637=CARTESIAN_POINT('',(51.2363981354663,44.9041895163455,22.9294657090004));
#35638=CARTESIAN_POINT('Ctrl Pts',(51.2481026219946,45.2483072643631,22.6294657090004));
#35639=CARTESIAN_POINT('Ctrl Pts',(51.2421409910059,45.0730323366345,22.783158980636));
#35640=CARTESIAN_POINT('Ctrl Pts',(51.2363981354663,44.9041895163455,22.9294657090004));
#35641=CARTESIAN_POINT('',(50.9442356670542,45.086384773026,22.6294657090004));
#35642=CARTESIAN_POINT('Ctrl Pts',(51.2363981354663,44.9041895163455,22.9294657090004));
#35643=CARTESIAN_POINT('Ctrl Pts',(51.0930473916193,44.9935843852776,22.783158980636));
#35644=CARTESIAN_POINT('Ctrl Pts',(50.9442356670542,45.0863847730261,22.6294657090004));
#35645=CARTESIAN_POINT('',(50.6658597152895,44.9231304191087,22.6294657090004));
#35646=CARTESIAN_POINT('Origin',(54.9397894030341,37.9543320991532,22.6294657090004));
#35647=CARTESIAN_POINT('',(50.6822429655713,44.5792036701988,22.9294657090004));
#35648=CARTESIAN_POINT('Ctrl Pts',(50.6658597152895,44.9231304191087,22.6294657090004));
#35649=CARTESIAN_POINT('Ctrl Pts',(50.674204454919,44.7479527759724,22.783158980636));
#35650=CARTESIAN_POINT('Ctrl Pts',(50.6822429655713,44.5792036701988,22.9294657090004));
#35651=CARTESIAN_POINT('',(50.3762020388334,44.7369787337131,22.6294657090004));
#35652=CARTESIAN_POINT('Ctrl Pts',(50.6822429655713,44.5792036701988,22.9294657090004));
#35653=CARTESIAN_POINT('Ctrl Pts',(50.5320826977793,44.6566166686521,22.783158980636));
#35654=CARTESIAN_POINT('Ctrl Pts',(50.3762020388334,44.7369787337131,22.6294657090004));
#35655=CARTESIAN_POINT('',(50.1120591055075,44.5515773708059,22.6294657090004));
#35656=CARTESIAN_POINT('Origin',(54.9397894030341,37.9543320991532,22.6294657090004));
#35657=CARTESIAN_POINT('',(50.1564210647719,44.2101303967736,22.9294657090004));
#35658=CARTESIAN_POINT('Ctrl Pts',(50.1120591055075,44.5515773708059,22.6294657090004));
#35659=CARTESIAN_POINT('Ctrl Pts',(50.1346546828898,44.3776627905745,22.783158980636));
#35660=CARTESIAN_POINT('Ctrl Pts',(50.1564210647719,44.2101303967736,22.9294657090004));
#35661=CARTESIAN_POINT('',(49.8385383315824,44.3424353001052,22.6294657090004));
#35662=CARTESIAN_POINT('Ctrl Pts',(50.1564210647719,44.2101303967736,22.9294657090004));
#35663=CARTESIAN_POINT('Ctrl Pts',(50.0004505648425,44.2750463540157,22.783158980636));
#35664=CARTESIAN_POINT('Ctrl Pts',(49.8385383315824,44.3424353001052,22.6294657090004));
#35665=CARTESIAN_POINT('',(49.5903862443362,44.1361207436891,22.6294657090004));
#35666=CARTESIAN_POINT('Origin',(54.9397894030341,37.9543320991532,22.6294657090004));
#35667=CARTESIAN_POINT('',(49.6624316910633,43.7994258178118,22.9294657090004));
#35668=CARTESIAN_POINT('Ctrl Pts',(49.5903862443362,44.1361207436891,22.6294657090004));
#35669=CARTESIAN_POINT('Ctrl Pts',(49.6270822896318,43.9646265992002,22.783158980636));
#35670=CARTESIAN_POINT('Ctrl Pts',(49.6624316910633,43.7994258178118,22.9294657090004));
#35671=CARTESIAN_POINT('',(49.3348226085648,43.9053800936577,22.6294657090004));
#35672=CARTESIAN_POINT('Ctrl Pts',(49.6624316910633,43.7994258178118,22.9294657090004));
#35673=CARTESIAN_POINT('Ctrl Pts',(49.5016889169402,43.8514127288577,22.783158980636));
#35674=CARTESIAN_POINT('Ctrl Pts',(49.3348226085648,43.9053800936577,22.6294657090004));
#35675=CARTESIAN_POINT('',(49.1043127785965,43.6795253330662,22.6294657090004));
#35676=CARTESIAN_POINT('Origin',(54.9397894030341,37.9543320991532,22.6294657090004));
#35677=CARTESIAN_POINT('',(49.2035622622253,43.349823104525,22.9294657090004));
#35678=CARTESIAN_POINT('Ctrl Pts',(49.1043127785965,43.6795253330662,22.6294657090004));
#35679=CARTESIAN_POINT('Ctrl Pts',(49.1548650856785,43.5115928895569,22.7831589806361));
#35680=CARTESIAN_POINT('Ctrl Pts',(49.2035622622253,43.349823104525,22.9294657090004));
#35681=CARTESIAN_POINT('',(48.8684070148099,43.4287216446606,22.6294657090004));
#35682=CARTESIAN_POINT('Ctrl Pts',(49.2035622622253,43.349823104525,22.9294657090004));
#35683=CARTESIAN_POINT('Ctrl Pts',(49.0391169305495,43.3885350050588,22.783158980636));
#35684=CARTESIAN_POINT('Ctrl Pts',(48.8684070148099,43.4287216446606,22.6294657090004));
#35685=CARTESIAN_POINT('',(48.6570734470067,43.184829706062,22.6294657090004));
#35686=CARTESIAN_POINT('Origin',(54.9397894030341,37.9543320991532,22.6294657090004));
#35687=CARTESIAN_POINT('',(48.7828664785984,42.8643142887907,22.9294657090004));
#35688=CARTESIAN_POINT('Ctrl Pts',(48.6570734470067,43.184829706062,22.6294657090004));
#35689=CARTESIAN_POINT('Ctrl Pts',(48.7211455986118,43.0215765262369,22.7831589806361));
#35690=CARTESIAN_POINT('Ctrl Pts',(48.7828664785984,42.8643142887908,22.9294657090004));
#35691=CARTESIAN_POINT('',(48.4423954691411,42.9156320364489,22.6294657090004));
#35692=CARTESIAN_POINT('Ctrl Pts',(48.7828664785984,42.8643142887907,22.9294657090004));
#35693=CARTESIAN_POINT('Ctrl Pts',(48.6158129459207,42.8894935575015,22.783158980636));
#35694=CARTESIAN_POINT('Ctrl Pts',(48.4423954691411,42.9156320364489,22.6294657090004));
#35695=CARTESIAN_POINT('',(48.251644553529,42.6553259804552,22.6294657090004));
#35696=CARTESIAN_POINT('Origin',(54.9397894030341,37.9543320991532,22.6294657090004));
#35697=CARTESIAN_POINT('',(48.4031440012129,42.3461303516745,22.9294657090004));
#35698=CARTESIAN_POINT('Ctrl Pts',(48.251644553529,42.6553259804551,22.6294657090004));
#35699=CARTESIAN_POINT('Ctrl Pts',(48.3288101600596,42.4978384872912,22.7831589806361));
#35700=CARTESIAN_POINT('Ctrl Pts',(48.4031440012129,42.3461303516745,22.9294657090004));
#35701=CARTESIAN_POINT('',(48.0596230081078,42.3695257957113,22.6294657090004));
#35702=CARTESIAN_POINT('Ctrl Pts',(48.4031440012129,42.3461303516745,22.9294657090004));
#35703=CARTESIAN_POINT('Ctrl Pts',(48.2345939812314,42.3576094246832,22.783158980636));
#35704=CARTESIAN_POINT('Ctrl Pts',(48.0596230081078,42.3695257957113,22.6294657090004));
#35705=CARTESIAN_POINT('',(47.8907241605586,42.0945379161777,22.6294657090004));
#35706=CARTESIAN_POINT('Origin',(54.9397894030341,37.9543320991532,22.6294657090004));
#35707=CARTESIAN_POINT('',(48.0669218205059,41.7987197217834,22.9294657090004));
#35708=CARTESIAN_POINT('Ctrl Pts',(47.8907241605586,42.0945379161777,22.6294657090004));
#35709=CARTESIAN_POINT('Ctrl Pts',(47.9804696976345,41.9438641629582,22.783158980636));
#35710=CARTESIAN_POINT('Ctrl Pts',(48.0669218205059,41.7987197217834,22.9294657090004));
#35711=CARTESIAN_POINT('',(47.7226369192852,41.7940371693788,22.6294657090004));
#35712=CARTESIAN_POINT('Ctrl Pts',(48.0669218205059,41.7987197217834,22.9294657090003));
#35713=CARTESIAN_POINT('Ctrl Pts',(47.8979969857948,41.7964222077531,22.783158980636));
#35714=CARTESIAN_POINT('Ctrl Pts',(47.7226369192852,41.7940371693788,22.6294657090003));
#35715=CARTESIAN_POINT('',(47.5767141337629,41.5061974652738,22.6294657090004));
#35716=CARTESIAN_POINT('Origin',(54.9397894030341,37.9543320991532,22.6294657090004));
#35717=CARTESIAN_POINT('',(47.7764374396173,41.2257253265431,22.9294657090004));
#35718=CARTESIAN_POINT('Ctrl Pts',(47.5767141337629,41.5061974652738,22.6294657090004));
#35719=CARTESIAN_POINT('Ctrl Pts',(47.678442359642,41.363340160967,22.783158980636));
#35720=CARTESIAN_POINT('Ctrl Pts',(47.7764374396173,41.225725326543,22.9294657090003));
#35721=CARTESIAN_POINT('',(47.4336797894956,41.1929959393107,22.6294657090004));
#35722=CARTESIAN_POINT('Ctrl Pts',(47.7764374396173,41.2257253265431,22.9294657090004));
#35723=CARTESIAN_POINT('Ctrl Pts',(47.6082619570809,41.2096665150506,22.783158980636));
#35724=CARTESIAN_POINT('Ctrl Pts',(47.4336797894956,41.1929959393107,22.6294657090004));
#35725=CARTESIAN_POINT('',(47.3117041580624,40.8942199363749,22.6294657090004));
#35726=CARTESIAN_POINT('Origin',(54.9397894030341,37.9543320991532,22.6294657090004));
#35727=CARTESIAN_POINT('',(47.5336239841754,40.6309603491163,22.9294657090004));
#35728=CARTESIAN_POINT('Ctrl Pts',(47.3117041580624,40.8942199363749,22.6294657090004));
#35729=CARTESIAN_POINT('Ctrl Pts',(47.4247380881853,40.7601297727712,22.7831589806361));
#35730=CARTESIAN_POINT('Ctrl Pts',(47.5336239841754,40.6309603491163,22.9294657090004));
#35731=CARTESIAN_POINT('',(47.1946745807631,40.5704019357283,22.6294657090004));
#35732=CARTESIAN_POINT('Ctrl Pts',(47.5336239841754,40.6309603491163,22.9294657090004));
#35733=CARTESIAN_POINT('Ctrl Pts',(47.367317033903,40.6012471089026,22.7831589806361));
#35734=CARTESIAN_POINT('Ctrl Pts',(47.1946745807631,40.5704019357283,22.6294657090004));
#35735=CARTESIAN_POINT('',(47.0974578311216,40.2626779389666,22.6294657090004));
#35736=CARTESIAN_POINT('Origin',(54.9397894030341,37.9543320991532,22.6294657090004));
#35737=CARTESIAN_POINT('',(47.3400973376647,40.0183828522986,22.9294657090004));
#35738=CARTESIAN_POINT('Ctrl Pts',(47.0974578311216,40.2626779389666,22.6294657090004));
#35739=CARTESIAN_POINT('Ctrl Pts',(47.2210452433328,40.1382472639815,22.783158980636));
#35740=CARTESIAN_POINT('Ctrl Pts',(47.3400973376646,40.0183828522986,22.9294657090004));
#35741=CARTESIAN_POINT('',(47.0072118333189,39.9303984190046,22.6294657090004));
#35742=CARTESIAN_POINT('Ctrl Pts',(47.3400973376647,40.0183828522986,22.9294657090004));
#35743=CARTESIAN_POINT('Ctrl Pts',(47.1767656649717,39.9752129200749,22.783158980636));
#35744=CARTESIAN_POINT('Ctrl Pts',(47.0072118333189,39.9303984190046,22.6294657090004));
#35745=CARTESIAN_POINT('',(46.9354009268983,39.6157742808447,22.6294657090004));
#35746=CARTESIAN_POINT('Origin',(54.9397894030341,37.9543320991532,22.6294657090004));
#35747=CARTESIAN_POINT('',(47.197145387988,39.3920694382632,22.9294657090004));
#35748=CARTESIAN_POINT('Ctrl Pts',(46.9354009268983,39.6157742808447,22.6294657090004));
#35749=CARTESIAN_POINT('Ctrl Pts',(47.0687193673599,39.5018311600905,22.7831589806361));
#35750=CARTESIAN_POINT('Ctrl Pts',(47.1971453879881,39.3920694382632,22.9294657090004));
#35751=CARTESIAN_POINT('',(46.872539080818,39.2772445069503,22.6294657090004));
#35752=CARTESIAN_POINT('Ctrl Pts',(47.197145387988,39.3920694382632,22.9294657090004));
#35753=CARTESIAN_POINT('Ctrl Pts',(47.0378759382083,39.3357301028059,22.783158980636));
#35754=CARTESIAN_POINT('Ctrl Pts',(46.872539080818,39.2772445069503,22.6294657090004));
#35755=CARTESIAN_POINT('',(46.8266119073525,38.9578139991222,22.6294657090004));
#35756=CARTESIAN_POINT('Origin',(54.9397894030341,37.9543320991532,22.6294657090004));
#35757=CARTESIAN_POINT('',(47.1057194567852,38.7561881194459,22.9294657090004));
#35758=CARTESIAN_POINT('Ctrl Pts',(46.8266119073525,38.9578139991222,22.6294657090004));
#35759=CARTESIAN_POINT('Ctrl Pts',(46.9687741638393,38.8551167052684,22.783158980636));
#35760=CARTESIAN_POINT('Ctrl Pts',(47.1057194567852,38.7561881194459,22.9294657090004));
#35761=CARTESIAN_POINT('',(46.7915525482088,38.6152868310873,22.6294657090004));
#35762=CARTESIAN_POINT('Ctrl Pts',(47.1057194567852,38.7561881194459,22.9294657090004));
#35763=CARTESIAN_POINT('Ctrl Pts',(46.9515721418295,38.6870543097372,22.783158980636));
#35764=CARTESIAN_POINT('Ctrl Pts',(46.7915525482088,38.6152868310873,22.6294657090004));
#35765=CARTESIAN_POINT('',(46.7718147454605,38.2931757109183,22.6294657090004));
#35766=CARTESIAN_POINT('Origin',(54.9397894030341,37.9543320991532,22.6294657090004));
#35767=CARTESIAN_POINT('Ctrl Pts',(46.7718147454605,38.2931757109183,22.6294657090004));
#35768=CARTESIAN_POINT('Ctrl Pts',(46.9218747516106,38.2024076775115,22.783158980636));
#35769=CARTESIAN_POINT('Ctrl Pts',(47.0664279685441,38.1149705811105,22.9294657090004));
#35770=CARTESIAN_POINT('Origin',(54.9397894030341,37.9543320991532,8.12867690713751));
#35771=CARTESIAN_POINT('',(56.9397894030341,37.9543320991532,8.12867690713751));
#35772=CARTESIAN_POINT('Origin',(54.9397894030341,37.9543320991532,8.12867690713751));
#35773=CARTESIAN_POINT('',(53.7817123633608,46.0468893322027,35.0304657090004));
#35774=CARTESIAN_POINT('',(54.1020132538699,46.0862910343601,35.0304657090004));
#35775=CARTESIAN_POINT('Origin',(54.9397894030341,37.9543320991532,8.12867690713751));
#35776=CARTESIAN_POINT('',(53.4419707382517,45.9909460781514,35.0304657090004));
#35777=CARTESIAN_POINT('',(53.1259472270462,45.9255679858026,35.0304657090004));
#35778=CARTESIAN_POINT('Origin',(54.9397894030341,37.9543320991532,8.12867690713751));
#35779=CARTESIAN_POINT('',(52.791895958725,45.8421187818605,35.0304657090004));
#35780=CARTESIAN_POINT('',(52.4822529111499,45.7511993797382,35.0304657090004));
#35781=CARTESIAN_POINT('Origin',(54.9397894030341,37.9543320991532,8.12867690713751));
#35782=CARTESIAN_POINT('',(52.1561150556927,45.6407995665893,35.0304657090004));
#35783=CARTESIAN_POINT('',(51.8549130951421,45.5249439083141,35.0304657090004));
#35784=CARTESIAN_POINT('Origin',(54.9397894030341,37.9543320991532,8.12867690713751));
#35785=CARTESIAN_POINT('',(51.5388590461679,45.3883281785002,35.0304657090004));
#35786=CARTESIAN_POINT('',(51.2481026219946,45.2483072643631,35.0304657090004));
#35787=CARTESIAN_POINT('Origin',(54.9397894030341,37.9543320991532,8.12867690713751));
#35788=CARTESIAN_POINT('',(50.9442356670542,45.086384773026,35.0304657090004));
#35789=CARTESIAN_POINT('',(50.6658597152895,44.9231304191087,35.0304657090004));
#35790=CARTESIAN_POINT('Origin',(54.9397894030341,37.9543320991532,8.12867690713751));
#35791=CARTESIAN_POINT('',(50.3762020388334,44.7369787337131,35.0304657090004));
#35792=CARTESIAN_POINT('',(50.1120591055075,44.5515773708059,35.0304657090004));
#35793=CARTESIAN_POINT('Origin',(54.9397894030341,37.9543320991532,8.12867690713751));
#35794=CARTESIAN_POINT('',(49.8385383315824,44.3424353001052,35.0304657090004));
#35795=CARTESIAN_POINT('',(49.5903862443362,44.1361207436891,35.0304657090004));
#35796=CARTESIAN_POINT('Origin',(54.9397894030341,37.9543320991532,8.12867690713751));
#35797=CARTESIAN_POINT('',(49.3348226085648,43.9053800936577,35.0304657090004));
#35798=CARTESIAN_POINT('',(49.1043127785965,43.6795253330662,35.0304657090004));
#35799=CARTESIAN_POINT('Origin',(54.9397894030341,37.9543320991532,8.12867690713751));
#35800=CARTESIAN_POINT('',(48.8684070148099,43.4287216446606,35.0304657090004));
#35801=CARTESIAN_POINT('',(48.6570734470067,43.184829706062,35.0304657090004));
#35802=CARTESIAN_POINT('Origin',(54.9397894030341,37.9543320991532,8.12867690713751));
#35803=CARTESIAN_POINT('',(48.4423954691411,42.9156320364489,35.0304657090004));
#35804=CARTESIAN_POINT('',(48.251644553529,42.6553259804552,35.0304657090004));
#35805=CARTESIAN_POINT('Origin',(54.9397894030341,37.9543320991532,8.12867690713751));
#35806=CARTESIAN_POINT('',(48.0596230081078,42.3695257957113,35.0304657090004));
#35807=CARTESIAN_POINT('',(47.8907241605586,42.0945379161777,35.0304657090004));
#35808=CARTESIAN_POINT('Origin',(54.9397894030341,37.9543320991532,8.12867690713751));
#35809=CARTESIAN_POINT('',(47.7226369192852,41.7940371693788,35.0304657090004));
#35810=CARTESIAN_POINT('',(47.5767141337629,41.5061974652738,35.0304657090004));
#35811=CARTESIAN_POINT('Origin',(54.9397894030341,37.9543320991532,8.12867690713751));
#35812=CARTESIAN_POINT('',(47.4336797894956,41.1929959393107,35.0304657090004));
#35813=CARTESIAN_POINT('',(47.3117041580624,40.8942199363749,35.0304657090004));
#35814=CARTESIAN_POINT('Origin',(54.9397894030341,37.9543320991532,8.12867690713751));
#35815=CARTESIAN_POINT('',(47.1946745807631,40.5704019357283,35.0304657090004));
#35816=CARTESIAN_POINT('',(47.0974578311216,40.2626779389666,35.0304657090004));
#35817=CARTESIAN_POINT('Origin',(54.9397894030341,37.9543320991532,8.12867690713751));
#35818=CARTESIAN_POINT('',(47.0072118333189,39.9303984190046,35.0304657090004));
#35819=CARTESIAN_POINT('',(46.9354009268983,39.6157742808447,35.0304657090004));
#35820=CARTESIAN_POINT('Origin',(54.9397894030341,37.9543320991532,8.12867690713751));
#35821=CARTESIAN_POINT('',(46.872539080818,39.2772445069503,35.0304657090004));
#35822=CARTESIAN_POINT('',(46.8266119073525,38.9578139991222,35.0304657090004));
#35823=CARTESIAN_POINT('Origin',(54.9397894030341,37.9543320991532,8.12867690713751));
#35824=CARTESIAN_POINT('',(46.7915525482088,38.6152868310873,35.0304657090004));
#35825=CARTESIAN_POINT('',(46.7718147454605,38.2931757109183,35.0304657090004));
#35826=CARTESIAN_POINT('Origin',(54.9397894030341,37.9543320991532,8.12867690713751));
#35827=CARTESIAN_POINT('',(46.764791187504,37.9489306105331,35.0304657090004));
#35828=CARTESIAN_POINT('',(46.7713741072936,37.6262824743834,35.0304657090004));
#35829=CARTESIAN_POINT('Origin',(54.9397894030341,37.9543320991532,8.12867690713751));
#35830=CARTESIAN_POINT('',(46.7924330911438,37.2826103359946,35.0304657090004));
#35831=CARTESIAN_POINT('',(46.8252929252262,36.961572353977,35.0304657090004));
#35832=CARTESIAN_POINT('Origin',(54.9397894030341,37.9543320991532,8.12867690713751));
#35833=CARTESIAN_POINT('',(46.8742943068201,36.6207602589635,35.0304657090004));
#35834=CARTESIAN_POINT('',(46.9332123784209,36.3034688858808,35.0304657090004));
#35835=CARTESIAN_POINT('Origin',(54.9397894030341,37.9543320991532,8.12867690713751));
#35836=CARTESIAN_POINT('',(47.0098300616486,35.967784882505,35.0304657090004));
#35837=CARTESIAN_POINT('',(47.0944142807223,35.6563516400958,35.0304657090004));
#35838=CARTESIAN_POINT('Origin',(54.9397894030341,37.9543320991532,8.12867690713751));
#35839=CARTESIAN_POINT('',(47.1981383875429,35.3280296500161,35.0304657090004));
#35840=CARTESIAN_POINT('',(47.3078258600668,35.0245270751256,35.0304657090004));
#35841=CARTESIAN_POINT('Origin',(54.9397894030341,37.9543320991532,8.12867690713751));
#35842=CARTESIAN_POINT('',(47.4379661236628,34.7057520270169,35.0304657090004));
#35843=CARTESIAN_POINT('',(47.5720268976044,34.4121998792066,35.0304657090004));
#35844=CARTESIAN_POINT('Origin',(54.9397894030341,37.9543320991532,8.12867690713751));
#35845=CARTESIAN_POINT('',(47.7277172559931,34.1050931684197,35.0304657090004));
#35846=CARTESIAN_POINT('',(47.8852591790204,33.8234449888006,35.0304657090004));
#35847=CARTESIAN_POINT('Origin',(54.9397894030341,37.9543320991532,8.12867690713751));
#35848=CARTESIAN_POINT('',(48.0654635385539,33.5300503598268,35.0304657090004));
#35849=CARTESIAN_POINT('',(48.2454381951617,33.2621804705657,35.0304657090004));
#35850=CARTESIAN_POINT('Origin',(54.9397894030341,37.9543320991532,8.12867690713751));
#35851=CARTESIAN_POINT('',(48.4489573255588,32.984450416254,35.0304657090004));
#35852=CARTESIAN_POINT('',(48.6501670141011,32.7321414472684,35.0304657090004));
#35853=CARTESIAN_POINT('Origin',(54.9397894030341,37.9543320991532,8.12867690713751));
#35854=CARTESIAN_POINT('',(48.8756465291274,32.4719242153081,35.0304657090004));
#35855=CARTESIAN_POINT('',(49.0967522323243,32.2368552411587,35.0304657090004));
#35856=CARTESIAN_POINT('Origin',(54.9397894030341,37.9543320991532,8.12867690713751));
#35857=CARTESIAN_POINT('',(49.3426916030088,31.9958825342957,35.0304657090004));
#35858=CARTESIAN_POINT('',(49.5822218988852,31.7796179002216,35.0304657090004));
#35859=CARTESIAN_POINT('Origin',(54.9397894030341,37.9543320991532,8.12867690713751));
#35860=CARTESIAN_POINT('',(49.8469844392931,31.5594933520623,35.0304657090004));
#35861=CARTESIAN_POINT('',(50.1033452932499,31.3634722635223,35.0304657090004));
#35862=CARTESIAN_POINT('Origin',(54.9397894030341,37.9543320991532,8.12867690713751));
#35863=CARTESIAN_POINT('',(50.3851690523575,31.1656607666167,35.0304657090004));
#35864=CARTESIAN_POINT('',(50.656654425208,30.9911877116138,35.0304657090004));
#35865=CARTESIAN_POINT('Origin',(54.9397894030341,37.9543320991532,8.12867690713751));
#35866=CARTESIAN_POINT('',(50.9536639123962,30.8170056688373,35.0304657090004));
#35867=CARTESIAN_POINT('',(51.2384671137761,30.6652417367663,35.0304657090004));
#35868=CARTESIAN_POINT('Origin',(54.9397894030341,37.9543320991532,8.12867690713751));
#35869=CARTESIAN_POINT('',(51.5486857799107,30.5158483008756,35.0304657090004));
#35870=CARTESIAN_POINT('',(51.844911491504,30.3878034556653,35.0304657090004));
#35871=CARTESIAN_POINT('Origin',(54.9397894030341,37.9543320991532,8.12867690713751));
#35872=CARTESIAN_POINT('',(52.1662748825443,30.264192815328,35.0304657090004));
#35873=CARTESIAN_POINT('',(52.4719517711141,30.1607191742974,35.0304657090004));
#35874=CARTESIAN_POINT('Origin',(54.9397894030341,37.9543320991532,8.12867690713751));
#35875=CARTESIAN_POINT('',(52.8023212667141,30.0637139379306,35.0304657090004));
#35876=CARTESIAN_POINT('',(53.1154151030002,29.9855001010888,35.0304657090004));
#35877=CARTESIAN_POINT('Origin',(54.9397894030341,37.9543320991532,8.12867690713751));
#35878=CARTESIAN_POINT('',(53.4525921486737,29.9157458225357,35.0304657090004));
#35879=CARTESIAN_POINT('',(53.7710193448524,29.8633122900625,35.0304657090004));
#35880=CARTESIAN_POINT('Origin',(54.9397894030341,37.9543320991532,8.12867690713751));
#35881=CARTESIAN_POINT('',(54.1127600829908,29.8212731725384,35.0304657090004));
#35882=CARTESIAN_POINT('',(54.4344015586084,29.7949688809415,35.0304657090004));
#35883=CARTESIAN_POINT('Origin',(54.9397894030341,37.9543320991532,8.12867690713751));
#35884=CARTESIAN_POINT('',(54.7784317609826,29.7809246878375,35.0304657090004));
#35885=CARTESIAN_POINT('',(55.1011470450858,29.7809246878375,35.0304657090004));
#35886=CARTESIAN_POINT('Origin',(54.9397894030341,37.9543320991532,8.12867690713751));
#35887=CARTESIAN_POINT('',(55.44517724746,29.7949688809415,35.0304657090004));
#35888=CARTESIAN_POINT('',(55.7668187230776,29.8212731725384,35.0304657090004));
#35889=CARTESIAN_POINT('Origin',(54.9397894030341,37.9543320991532,8.12867690713751));
#35890=CARTESIAN_POINT('',(56.108559461216,29.8633122900625,35.0304657090004));
#35891=CARTESIAN_POINT('',(56.4269866573947,29.9157458225358,35.0304657090004));
#35892=CARTESIAN_POINT('Origin',(54.9397894030341,37.9543320991532,8.12867690713751));
#35893=CARTESIAN_POINT('',(56.7641637030682,29.9855001010888,35.0304657090004));
#35894=CARTESIAN_POINT('',(57.0772575393543,30.0637139379306,35.0304657090004));
#35895=CARTESIAN_POINT('Origin',(54.9397894030341,37.9543320991532,8.12867690713751));
#35896=CARTESIAN_POINT('',(57.4076270349543,30.1607191742974,35.0304657090004));
#35897=CARTESIAN_POINT('',(57.7133039235241,30.264192815328,35.0304657090004));
#35898=CARTESIAN_POINT('Origin',(54.9397894030341,37.9543320991532,8.12867690713751));
#35899=CARTESIAN_POINT('',(58.0346673145645,30.3878034556654,35.0304657090004));
#35900=CARTESIAN_POINT('',(58.3308930261577,30.5158483008756,35.0304657090004));
#35901=CARTESIAN_POINT('Origin',(54.9397894030341,37.9543320991532,8.12867690713751));
#35902=CARTESIAN_POINT('',(58.6411116922923,30.6652417367664,35.0304657090004));
#35903=CARTESIAN_POINT('',(58.9259148936722,30.8170056688373,35.0304657090004));
#35904=CARTESIAN_POINT('Origin',(54.9397894030341,37.9543320991532,8.12867690713751));
#35905=CARTESIAN_POINT('',(59.2229243808604,30.9911877116138,35.0304657090004));
#35906=CARTESIAN_POINT('',(59.4944097537108,31.1656607666168,35.0304657090004));
#35907=CARTESIAN_POINT('Origin',(54.9397894030341,37.9543320991532,8.12867690713751));
#35908=CARTESIAN_POINT('',(59.7762335128185,31.3634722635224,35.0304657090004));
#35909=CARTESIAN_POINT('',(60.0325943667752,31.5594933520624,35.0304657090004));
#35910=CARTESIAN_POINT('Origin',(54.9397894030341,37.9543320991532,8.12867690713751));
#35911=CARTESIAN_POINT('',(60.2973569071831,31.7796179002217,35.0304657090004));
#35912=CARTESIAN_POINT('',(60.5368872030596,31.9958825342957,35.0304657090004));
#35913=CARTESIAN_POINT('Origin',(54.9397894030341,37.9543320991532,8.12867690713751));
#35914=CARTESIAN_POINT('',(60.7828265737441,32.2368552411588,35.0304657090004));
#35915=CARTESIAN_POINT('',(61.0039322769409,32.4719242153082,35.0304657090004));
#35916=CARTESIAN_POINT('Origin',(54.9397894030341,37.9543320991532,8.12867690713751));
#35917=CARTESIAN_POINT('',(61.2294117919672,32.7321414472685,35.0304657090004));
#35918=CARTESIAN_POINT('',(61.4306214805095,32.9844504162541,35.0304657090004));
#35919=CARTESIAN_POINT('Origin',(54.9397894030341,37.9543320991532,8.12867690713751));
#35920=CARTESIAN_POINT('',(61.6341406109067,33.2621804705658,35.0304657090004));
#35921=CARTESIAN_POINT('',(61.8141152675145,33.5300503598269,35.0304657090004));
#35922=CARTESIAN_POINT('Origin',(54.9397894030341,37.9543320991532,8.12867690713751));
#35923=CARTESIAN_POINT('',(61.9943196270479,33.8234449888007,35.0304657090004));
#35924=CARTESIAN_POINT('',(62.1518615500752,34.1050931684198,35.0304657090004));
#35925=CARTESIAN_POINT('Origin',(54.9397894030341,37.9543320991532,8.12867690713751));
#35926=CARTESIAN_POINT('',(62.3075519084639,34.4121998792067,35.0304657090004));
#35927=CARTESIAN_POINT('',(62.4416126824056,34.705752027017,35.0304657090004));
#35928=CARTESIAN_POINT('Origin',(54.9397894030341,37.9543320991532,8.12867690713751));
#35929=CARTESIAN_POINT('',(62.5717529460015,35.0245270751257,35.0304657090004));
#35930=CARTESIAN_POINT('',(62.6814404185254,35.3280296500162,35.0304657090004));
#35931=CARTESIAN_POINT('Origin',(54.9397894030341,37.9543320991532,8.12867690713751));
#35932=CARTESIAN_POINT('',(62.785164525346,35.6563516400959,35.0304657090004));
#35933=CARTESIAN_POINT('',(62.8697487444197,35.9677848825051,35.0304657090004));
#35934=CARTESIAN_POINT('Origin',(54.9397894030341,37.9543320991532,8.12867690713751));
#35935=CARTESIAN_POINT('',(62.9463664276474,36.3034688858809,35.0304657090004));
#35936=CARTESIAN_POINT('',(63.0052844992482,36.6207602589636,35.0304657090004));
#35937=CARTESIAN_POINT('Origin',(54.9397894030341,37.9543320991532,8.12867690713751));
#35938=CARTESIAN_POINT('',(63.0542858808421,36.9615723539771,35.0304657090004));
#35939=CARTESIAN_POINT('',(63.0871457149245,37.2826103359947,35.0304657090004));
#35940=CARTESIAN_POINT('Origin',(54.9397894030341,37.9543320991532,8.12867690713751));
#35941=CARTESIAN_POINT('',(63.1082046987747,37.6262824743835,35.0304657090004));
#35942=CARTESIAN_POINT('',(63.1147876185643,37.9489306105332,35.0304657090004));
#35943=CARTESIAN_POINT('Origin',(54.9397894030341,37.9543320991532,8.12867690713751));
#35944=CARTESIAN_POINT('',(63.1077640606078,38.2931757109184,35.0304657090004));
#35945=CARTESIAN_POINT('',(63.0880262578595,38.6152868310874,35.0304657090004));
#35946=CARTESIAN_POINT('Origin',(54.9397894030341,37.9543320991532,8.12867690713751));
#35947=CARTESIAN_POINT('',(63.0529668987158,38.9578139991223,35.0304657090004));
#35948=CARTESIAN_POINT('',(63.0070397252503,39.2772445069504,35.0304657090004));
#35949=CARTESIAN_POINT('Origin',(54.9397894030341,37.9543320991532,8.12867690713751));
#35950=CARTESIAN_POINT('',(62.94417787917,39.6157742808448,35.0304657090004));
#35951=CARTESIAN_POINT('',(62.8723669727493,39.9303984190047,35.0304657090004));
#35952=CARTESIAN_POINT('Origin',(54.9397894030341,37.9543320991532,8.12867690713751));
#35953=CARTESIAN_POINT('',(62.7821209749467,40.2626779389667,35.0304657090004));
#35954=CARTESIAN_POINT('',(62.6849042253051,40.5704019357284,35.0304657090004));
#35955=CARTESIAN_POINT('Origin',(54.9397894030341,37.9543320991532,8.12867690713751));
#35956=CARTESIAN_POINT('',(62.5678746480059,40.894219936375,35.0304657090004));
#35957=CARTESIAN_POINT('',(62.4458990165727,41.1929959393108,35.0304657090004));
#35958=CARTESIAN_POINT('Origin',(54.9397894030341,37.9543320991532,8.12867690713751));
#35959=CARTESIAN_POINT('',(62.3028646723053,41.5061974652739,35.0304657090004));
#35960=CARTESIAN_POINT('',(62.1569418867831,41.7940371693789,35.0304657090004));
#35961=CARTESIAN_POINT('Origin',(54.9397894030341,37.9543320991532,8.12867690713751));
#35962=CARTESIAN_POINT('',(61.9888546455096,42.0945379161778,35.0304657090004));
#35963=CARTESIAN_POINT('',(61.8199557979604,42.3695257957114,35.0304657090004));
#35964=CARTESIAN_POINT('Origin',(54.9397894030341,37.9543320991532,8.12867690713751));
#35965=CARTESIAN_POINT('',(61.6279342525392,42.6553259804552,35.0304657090004));
#35966=CARTESIAN_POINT('',(61.4371833369271,42.915632036449,35.0304657090004));
#35967=CARTESIAN_POINT('Origin',(54.9397894030341,37.9543320991532,8.12867690713751));
#35968=CARTESIAN_POINT('',(61.2225053590615,43.184829706062,35.0304657090004));
#35969=CARTESIAN_POINT('',(61.0111717912583,43.4287216446607,35.0304657090004));
#35970=CARTESIAN_POINT('Origin',(54.9397894030341,37.9543320991532,8.12867690713751));
#35971=CARTESIAN_POINT('',(60.7752660274717,43.6795253330662,35.0304657090004));
#35972=CARTESIAN_POINT('',(60.5447561975034,43.9053800936578,35.0304657090004));
#35973=CARTESIAN_POINT('Origin',(54.9397894030341,37.9543320991532,8.12867690713751));
#35974=CARTESIAN_POINT('',(60.289192561732,44.1361207436891,35.0304657090004));
#35975=CARTESIAN_POINT('',(60.0410404744858,44.3424353001052,35.0304657090004));
#35976=CARTESIAN_POINT('Origin',(54.9397894030341,37.9543320991532,8.12867690713751));
#35977=CARTESIAN_POINT('',(59.7675197005607,44.551577370806,35.0304657090004));
#35978=CARTESIAN_POINT('',(59.5033767672348,44.7369787337132,35.0304657090004));
#35979=CARTESIAN_POINT('Origin',(54.9397894030341,37.9543320991532,8.12867690713751));
#35980=CARTESIAN_POINT('',(59.2137190907787,44.9231304191088,35.0304657090004));
#35981=CARTESIAN_POINT('',(58.935343139014,45.0863847730261,35.0304657090004));
#35982=CARTESIAN_POINT('Origin',(54.9397894030341,37.9543320991532,8.12867690713751));
#35983=CARTESIAN_POINT('',(58.6314761840736,45.2483072643631,35.0304657090004));
#35984=CARTESIAN_POINT('',(58.3407197599002,45.3883281785002,35.0304657090004));
#35985=CARTESIAN_POINT('Origin',(54.9397894030341,37.9543320991532,8.12867690713751));
#35986=CARTESIAN_POINT('',(58.024665710926,45.5249439083142,35.0304657090004));
#35987=CARTESIAN_POINT('',(57.7234637503755,45.6407995665893,35.0304657090004));
#35988=CARTESIAN_POINT('Origin',(54.9397894030341,37.9543320991532,8.12867690713751));
#35989=CARTESIAN_POINT('',(57.3973258949183,45.7511993797383,35.0304657090004));
#35990=CARTESIAN_POINT('',(57.0876828473432,45.8421187818605,35.0304657090004));
#35991=CARTESIAN_POINT('Origin',(54.9397894030341,37.9543320991532,8.12867690713751));
#35992=CARTESIAN_POINT('',(56.753631579022,45.9255679858027,35.0304657090004));
#35993=CARTESIAN_POINT('',(56.4376080678165,45.9909460781515,35.0304657090004));
#35994=CARTESIAN_POINT('Origin',(54.9397894030341,37.9543320991532,8.12867690713751));
#35995=CARTESIAN_POINT('',(56.0978664427074,46.0468893322027,35.0304657090004));
#35996=CARTESIAN_POINT('',(55.7775655521983,46.0862910343602,35.0304657090004));
#35997=CARTESIAN_POINT('Origin',(54.9397894030341,37.9543320991532,8.12867690713751));
#35998=CARTESIAN_POINT('',(54.4451843113051,46.1143560453948,35.0304657090004));
#35999=CARTESIAN_POINT('',(54.7676310315374,46.1275191455338,35.0304657090004));
#36000=CARTESIAN_POINT('Origin',(54.9397894030341,39.9543320991532,23.0294657090004));
#36001=CARTESIAN_POINT('Origin',(54.9397894030341,37.9543320991532,8.12867690713751));
#36002=CARTESIAN_POINT('',(55.4343944947631,46.1143560453948,35.0304657090004));
#36003=CARTESIAN_POINT('',(55.1119477745308,46.1275191455338,35.0304657090004));
#36004=CARTESIAN_POINT('Origin',(54.9397894030341,37.9543320991532,19.5294657090004));
#36005=CARTESIAN_POINT('Origin',(54.9397894030341,39.5643320991532,35.0294657090004));
#36006=CARTESIAN_POINT('Origin',(54.9397894030341,45.8293320991532,35.0304657090004));
#36007=CARTESIAN_POINT('',(54.9397894030341,45.8293320991532,35.0304657090004));
#36008=CARTESIAN_POINT('Origin',(54.9397894030341,45.8293320991532,35.0304657090004));
#36009=CARTESIAN_POINT('Origin',(54.297903795101,45.803128686295,35.0304657090004));
#36010=CARTESIAN_POINT('',(54.297903795101,45.803128686295,35.0304657090004));
#36011=CARTESIAN_POINT('Origin',(54.297903795101,45.803128686295,35.0304657090004));
#36012=CARTESIAN_POINT('Origin',(55.5816750109672,45.803128686295,35.0304657090004));
#36013=CARTESIAN_POINT('',(55.5816750109672,45.803128686295,35.0304657090004));
#36014=CARTESIAN_POINT('Origin',(55.5816750109672,45.803128686295,35.0304657090004));
#36015=CARTESIAN_POINT('Origin',(56.2192889760832,45.7246928271096,35.0304657090004));
#36016=CARTESIAN_POINT('',(56.2192889760832,45.7246928271096,35.0304657090004));
#36017=CARTESIAN_POINT('Origin',(56.2192889760832,45.7246928271096,35.0304657090004));
#36018=CARTESIAN_POINT('Origin',(56.8483880826431,45.594546499299,35.0304657090004));
#36019=CARTESIAN_POINT('',(56.8483880826431,45.594546499299,35.0304657090004));
#36020=CARTESIAN_POINT('Origin',(56.8483880826431,45.594546499299,35.0304657090004));
#36021=CARTESIAN_POINT('Origin',(57.4647857798868,45.413555805202,35.0304657090004));
#36022=CARTESIAN_POINT('',(57.4647857798868,45.413555805202,35.0304657090004));
#36023=CARTESIAN_POINT('Origin',(57.4647857798868,45.413555805202,35.0304657090004));
#36024=CARTESIAN_POINT('Origin',(58.0643800428377,45.1829252080266,35.0304657090004));
#36025=CARTESIAN_POINT('',(58.0643800428377,45.1829252080266,35.0304657090004));
#36026=CARTESIAN_POINT('Origin',(58.0643800428377,45.1829252080266,35.0304657090004));
#36027=CARTESIAN_POINT('Origin',(58.6431806706019,44.9041895163456,35.0304657090004));
#36028=CARTESIAN_POINT('',(58.6431806706019,44.9041895163456,35.0304657090004));
#36029=CARTESIAN_POINT('Origin',(58.6431806706019,44.9041895163456,35.0304657090004));
#36030=CARTESIAN_POINT('Origin',(59.1973358404969,44.5792036701988,35.0304657090004));
#36031=CARTESIAN_POINT('',(59.1973358404969,44.5792036701988,35.0304657090004));
#36032=CARTESIAN_POINT('Origin',(59.1973358404969,44.5792036701988,35.0304657090004));
#36033=CARTESIAN_POINT('Origin',(59.7231577412963,44.2101303967737,35.0304657090004));
#36034=CARTESIAN_POINT('',(59.7231577412963,44.2101303967737,35.0304657090004));
#36035=CARTESIAN_POINT('Origin',(59.7231577412963,44.2101303967737,35.0304657090004));
#36036=CARTESIAN_POINT('Origin',(60.2171471150049,43.7994258178119,35.0304657090004));
#36037=CARTESIAN_POINT('',(60.2171471150049,43.7994258178119,35.0304657090004));
#36038=CARTESIAN_POINT('Origin',(60.2171471150049,43.7994258178119,35.0304657090004));
#36039=CARTESIAN_POINT('Origin',(60.6760165438429,43.3498231045251,35.0304657090004));
#36040=CARTESIAN_POINT('',(60.6760165438429,43.3498231045251,35.0304657090004));
#36041=CARTESIAN_POINT('Origin',(60.6760165438429,43.3498231045251,35.0304657090004));
#36042=CARTESIAN_POINT('Origin',(61.0967123274698,42.8643142887908,35.0304657090004));
#36043=CARTESIAN_POINT('',(61.0967123274698,42.8643142887908,35.0304657090004));
#36044=CARTESIAN_POINT('Origin',(61.0967123274698,42.8643142887908,35.0304657090004));
#36045=CARTESIAN_POINT('Origin',(61.4764348048554,42.3461303516746,35.0304657090004));
#36046=CARTESIAN_POINT('',(61.4764348048554,42.3461303516746,35.0304657090004));
#36047=CARTESIAN_POINT('Origin',(61.4764348048554,42.3461303516746,35.0304657090004));
#36048=CARTESIAN_POINT('Origin',(61.8126569855623,41.7987197217835,35.0304657090004));
#36049=CARTESIAN_POINT('',(61.8126569855623,41.7987197217835,35.0304657090004));
#36050=CARTESIAN_POINT('Origin',(61.8126569855623,41.7987197217835,35.0304657090004));
#36051=CARTESIAN_POINT('Origin',(62.1031413664509,41.2257253265432,35.0304657090004));
#36052=CARTESIAN_POINT('',(62.1031413664509,41.2257253265432,35.0304657090004));
#36053=CARTESIAN_POINT('Origin',(62.1031413664509,41.2257253265432,35.0304657090004));
#36054=CARTESIAN_POINT('Origin',(62.3459548218929,40.6309603491164,35.0304657090004));
#36055=CARTESIAN_POINT('',(62.3459548218929,40.6309603491164,35.0304657090004));
#36056=CARTESIAN_POINT('Origin',(62.3459548218929,40.6309603491164,35.0304657090004));
#36057=CARTESIAN_POINT('Origin',(62.5394814684036,40.0183828522987,35.0304657090004));
#36058=CARTESIAN_POINT('',(62.5394814684036,40.0183828522987,35.0304657090004));
#36059=CARTESIAN_POINT('Origin',(62.5394814684036,40.0183828522987,35.0304657090004));
#36060=CARTESIAN_POINT('Origin',(62.6824334180802,39.3920694382633,35.0304657090004));
#36061=CARTESIAN_POINT('',(62.6824334180802,39.3920694382633,35.0304657090004));
#36062=CARTESIAN_POINT('Origin',(62.6824334180802,39.3920694382633,35.0304657090004));
#36063=CARTESIAN_POINT('Origin',(62.773859349283,38.756188119446,35.0304657090004));
#36064=CARTESIAN_POINT('',(62.773859349283,38.756188119446,35.0304657090004));
#36065=CARTESIAN_POINT('Origin',(62.773859349283,38.756188119446,35.0304657090004));
#36066=CARTESIAN_POINT('Origin',(62.8131508375241,38.1149705811106,35.0304657090004));
#36067=CARTESIAN_POINT('',(62.8131508375241,38.1149705811106,35.0304657090004));
#36068=CARTESIAN_POINT('Origin',(62.8131508375241,38.1149705811106,35.0304657090004));
#36069=CARTESIAN_POINT('Origin',(62.8000464044319,37.4726840201813,35.0304657090004));
#36070=CARTESIAN_POINT('',(62.8000464044319,37.4726840201813,35.0304657090004));
#36071=CARTESIAN_POINT('Origin',(62.8000464044319,37.4726840201813,35.0304657090004));
#36072=CARTESIAN_POINT('Origin',(62.7346332578465,36.8336027477512,35.0304657090004));
#36073=CARTESIAN_POINT('',(62.7346332578465,36.8336027477512,35.0304657090004));
#36074=CARTESIAN_POINT('Origin',(62.7346332578465,36.8336027477512,35.0304657090004));
#36075=CARTESIAN_POINT('Origin',(62.617346711466,36.2019797442473,35.0304657090004));
#36076=CARTESIAN_POINT('',(62.617346711466,36.2019797442473,35.0304657090004));
#36077=CARTESIAN_POINT('Origin',(62.617346711466,36.2019797442473,35.0304657090004));
#36078=CARTESIAN_POINT('Origin',(62.4489672879057,35.5820183565476,35.0304657090004));
#36079=CARTESIAN_POINT('',(62.4489672879057,35.5820183565476,35.0304657090004));
#36080=CARTESIAN_POINT('Origin',(62.4489672879057,35.5820183565476,35.0304657090004));
#36081=CARTESIAN_POINT('Origin',(62.2306155244487,34.9778443254007,35.0304657090004));
#36082=CARTESIAN_POINT('',(62.2306155244487,34.9778443254007,35.0304657090004));
#36083=CARTESIAN_POINT('Origin',(62.2306155244487,34.9778443254007,35.0304657090004));
#36084=CARTESIAN_POINT('Origin',(61.9637445160554,34.3934783293021,35.0304657090004));
#36085=CARTESIAN_POINT('',(61.9637445160554,34.3934783293021,35.0304657090004));
#36086=CARTESIAN_POINT('Origin',(61.9637445160554,34.3934783293021,35.0304657090004));
#36087=CARTESIAN_POINT('Origin',(61.6501302452559,33.8328092275425,35.0304657090004));
#36088=CARTESIAN_POINT('',(61.6501302452559,33.8328092275425,35.0304657090004));
#36089=CARTESIAN_POINT('Origin',(61.6501302452559,33.8328092275425,35.0304657090004));
#36090=CARTESIAN_POINT('Origin',(61.2918597632797,33.2995681804899,35.0304657090004));
#36091=CARTESIAN_POINT('',(61.2918597632797,33.2995681804899,35.0304657090004));
#36092=CARTESIAN_POINT('Origin',(61.2918597632797,33.2995681804899,35.0304657090004));
#36093=CARTESIAN_POINT('Origin',(60.891317301074,32.7973038193341,35.0304657090004));
#36094=CARTESIAN_POINT('',(60.891317301074,32.7973038193341,35.0304657090004));
#36095=CARTESIAN_POINT('Origin',(60.891317301074,32.7973038193341,35.0304657090004));
#36096=CARTESIAN_POINT('Origin',(60.4511684026397,32.3293586305308,35.0304657090004));
#36097=CARTESIAN_POINT('',(60.4511684026397,32.3293586305308,35.0304657090004));
#36098=CARTESIAN_POINT('Origin',(60.4511684026397,32.3293586305308,35.0304657090004));
#36099=CARTESIAN_POINT('Origin',(59.9743421862767,31.8988467121058,35.0304657090004));
#36100=CARTESIAN_POINT('',(59.9743421862767,31.8988467121058,35.0304657090004));
#36101=CARTESIAN_POINT('Origin',(59.9743421862767,31.8988467121058,35.0304657090004));
#36102=CARTESIAN_POINT('Origin',(59.4640118517838,31.5086330498468,35.0304657090004));
#36103=CARTESIAN_POINT('',(59.4640118517838,31.5086330498468,35.0304657090004));
#36104=CARTESIAN_POINT('Origin',(59.4640118517838,31.5086330498468,35.0304657090004));
#36105=CARTESIAN_POINT('Origin',(58.9235735633388,31.1613144512955,35.0304657090004));
#36106=CARTESIAN_POINT('',(58.9235735633388,31.1613144512955,35.0304657090004));
#36107=CARTESIAN_POINT('Origin',(58.9235735633388,31.1613144512955,35.0304657090004));
#36108=CARTESIAN_POINT('Origin',(58.356623848585,30.8592022644217,35.0304657090004));
#36109=CARTESIAN_POINT('',(58.356623848585,30.8592022644217,35.0304657090004));
#36110=CARTESIAN_POINT('Origin',(58.356623848585,30.8592022644217,35.0304657090004));
#36111=CARTESIAN_POINT('Origin',(57.766935664334,30.604306995984,35.0304657090004));
#36112=CARTESIAN_POINT('',(57.766935664334,30.604306995984,35.0304657090004));
#36113=CARTESIAN_POINT('Origin',(57.766935664334,30.604306995984,35.0304657090004));
#36114=CARTESIAN_POINT('Origin',(57.1584332881605,30.3983249319391,35.0304657090004));
#36115=CARTESIAN_POINT('',(57.1584332881605,30.3983249319391,35.0304657090004));
#36116=CARTESIAN_POINT('Origin',(57.1584332881605,30.3983249319391,35.0304657090004));
#36117=CARTESIAN_POINT('Origin',(56.5351662029818,30.2426268489385,35.0304657090004));
#36118=CARTESIAN_POINT('',(56.5351662029818,30.2426268489385,35.0304657090004));
#36119=CARTESIAN_POINT('Origin',(56.5351662029818,30.2426268489385,35.0304657090004));
#36120=CARTESIAN_POINT('Origin',(55.9012821484182,30.1382488920364,35.0304657090004));
#36121=CARTESIAN_POINT('',(55.9012821484182,30.1382488920364,35.0304657090004));
#36122=CARTESIAN_POINT('Origin',(55.9012821484182,30.1382488920364,35.0304657090004));
#36123=CARTESIAN_POINT('Origin',(55.2609995182692,30.0858856793146,35.0304657090004));
#36124=CARTESIAN_POINT('',(55.2609995182692,30.0858856793146,35.0304657090004));
#36125=CARTESIAN_POINT('Origin',(55.2609995182692,30.0858856793146,35.0304657090004));
#36126=CARTESIAN_POINT('Origin',(54.6185792877992,30.0858856793146,35.0304657090004));
#36127=CARTESIAN_POINT('',(54.6185792877992,30.0858856793146,35.0304657090004));
#36128=CARTESIAN_POINT('Origin',(54.6185792877992,30.0858856793146,35.0304657090004));
#36129=CARTESIAN_POINT('Origin',(53.9782966576502,30.1382488920364,35.0304657090004));
#36130=CARTESIAN_POINT('',(53.9782966576502,30.1382488920364,35.0304657090004));
#36131=CARTESIAN_POINT('Origin',(53.9782966576502,30.1382488920364,35.0304657090004));
#36132=CARTESIAN_POINT('Origin',(53.3444126030866,30.2426268489385,35.0304657090004));
#36133=CARTESIAN_POINT('',(53.3444126030866,30.2426268489385,35.0304657090004));
#36134=CARTESIAN_POINT('Origin',(53.3444126030866,30.2426268489385,35.0304657090004));
#36135=CARTESIAN_POINT('Origin',(52.7211455179079,30.398324931939,35.0304657090004));
#36136=CARTESIAN_POINT('',(52.7211455179079,30.398324931939,35.0304657090004));
#36137=CARTESIAN_POINT('Origin',(52.7211455179079,30.398324931939,35.0304657090004));
#36138=CARTESIAN_POINT('Origin',(52.1126431417343,30.6043069959839,35.0304657090004));
#36139=CARTESIAN_POINT('',(52.1126431417343,30.6043069959839,35.0304657090004));
#36140=CARTESIAN_POINT('Origin',(52.1126431417343,30.6043069959839,35.0304657090004));
#36141=CARTESIAN_POINT('Origin',(51.5229549574834,30.8592022644217,35.0304657090004));
#36142=CARTESIAN_POINT('',(51.5229549574834,30.8592022644217,35.0304657090004));
#36143=CARTESIAN_POINT('Origin',(51.5229549574834,30.8592022644217,35.0304657090004));
#36144=CARTESIAN_POINT('Origin',(50.9560052427296,31.1613144512955,35.0304657090004));
#36145=CARTESIAN_POINT('',(50.9560052427296,31.1613144512955,35.0304657090004));
#36146=CARTESIAN_POINT('Origin',(50.9560052427296,31.1613144512955,35.0304657090004));
#36147=CARTESIAN_POINT('Origin',(50.4155669542845,31.5086330498468,35.0304657090004));
#36148=CARTESIAN_POINT('',(50.4155669542845,31.5086330498468,35.0304657090004));
#36149=CARTESIAN_POINT('Origin',(50.4155669542845,31.5086330498468,35.0304657090004));
#36150=CARTESIAN_POINT('Origin',(49.9052366197917,31.8988467121057,35.0304657090004));
#36151=CARTESIAN_POINT('',(49.9052366197917,31.8988467121057,35.0304657090004));
#36152=CARTESIAN_POINT('Origin',(49.9052366197917,31.8988467121057,35.0304657090004));
#36153=CARTESIAN_POINT('Origin',(49.4284104034286,32.3293586305307,35.0304657090004));
#36154=CARTESIAN_POINT('',(49.4284104034286,32.3293586305307,35.0304657090004));
#36155=CARTESIAN_POINT('Origin',(49.4284104034286,32.3293586305307,35.0304657090004));
#36156=CARTESIAN_POINT('Origin',(48.9882615049944,32.7973038193341,35.0304657090004));
#36157=CARTESIAN_POINT('',(48.9882615049944,32.7973038193341,35.0304657090004));
#36158=CARTESIAN_POINT('Origin',(48.9882615049944,32.7973038193341,35.0304657090004));
#36159=CARTESIAN_POINT('Origin',(48.5877190427886,33.2995681804899,35.0304657090004));
#36160=CARTESIAN_POINT('',(48.5877190427886,33.2995681804899,35.0304657090004));
#36161=CARTESIAN_POINT('Origin',(48.5877190427886,33.2995681804899,35.0304657090004));
#36162=CARTESIAN_POINT('Origin',(48.2294485608124,33.8328092275424,35.0304657090004));
#36163=CARTESIAN_POINT('',(48.2294485608124,33.8328092275424,35.0304657090004));
#36164=CARTESIAN_POINT('Origin',(48.2294485608124,33.8328092275424,35.0304657090004));
#36165=CARTESIAN_POINT('Origin',(47.9158342900129,34.393478329302,35.0304657090004));
#36166=CARTESIAN_POINT('',(47.9158342900129,34.393478329302,35.0304657090004));
#36167=CARTESIAN_POINT('Origin',(47.9158342900129,34.393478329302,35.0304657090004));
#36168=CARTESIAN_POINT('Origin',(47.6489632816196,34.9778443254006,35.0304657090004));
#36169=CARTESIAN_POINT('',(47.6489632816196,34.9778443254006,35.0304657090004));
#36170=CARTESIAN_POINT('Origin',(47.6489632816196,34.9778443254006,35.0304657090004));
#36171=CARTESIAN_POINT('Origin',(47.4306115181626,35.5820183565475,35.0304657090004));
#36172=CARTESIAN_POINT('',(47.4306115181626,35.5820183565475,35.0304657090004));
#36173=CARTESIAN_POINT('Origin',(47.4306115181626,35.5820183565475,35.0304657090004));
#36174=CARTESIAN_POINT('Origin',(47.2622320946023,36.2019797442472,35.0304657090004));
#36175=CARTESIAN_POINT('',(47.2622320946023,36.2019797442472,35.0304657090004));
#36176=CARTESIAN_POINT('Origin',(47.2622320946023,36.2019797442472,35.0304657090004));
#36177=CARTESIAN_POINT('Origin',(47.1449455482218,36.8336027477511,35.0304657090004));
#36178=CARTESIAN_POINT('',(47.1449455482218,36.8336027477511,35.0304657090004));
#36179=CARTESIAN_POINT('Origin',(47.1449455482218,36.8336027477511,35.0304657090004));
#36180=CARTESIAN_POINT('Origin',(47.0795324016364,37.4726840201812,35.0304657090004));
#36181=CARTESIAN_POINT('',(47.0795324016364,37.4726840201812,35.0304657090004));
#36182=CARTESIAN_POINT('Origin',(47.0795324016364,37.4726840201812,35.0304657090004));
#36183=CARTESIAN_POINT('Origin',(47.0664279685441,38.1149705811105,35.0304657090004));
#36184=CARTESIAN_POINT('',(47.0664279685441,38.1149705811105,35.0304657090004));
#36185=CARTESIAN_POINT('Origin',(47.0664279685441,38.1149705811105,35.0304657090004));
#36186=CARTESIAN_POINT('Origin',(47.1057194567852,38.7561881194459,35.0304657090004));
#36187=CARTESIAN_POINT('',(47.1057194567852,38.7561881194459,35.0304657090004));
#36188=CARTESIAN_POINT('Origin',(47.1057194567852,38.7561881194459,35.0304657090004));
#36189=CARTESIAN_POINT('Origin',(47.197145387988,39.3920694382632,35.0304657090004));
#36190=CARTESIAN_POINT('',(47.197145387988,39.3920694382632,35.0304657090004));
#36191=CARTESIAN_POINT('Origin',(47.197145387988,39.3920694382632,35.0304657090004));
#36192=CARTESIAN_POINT('Origin',(47.3400973376647,40.0183828522986,35.0304657090004));
#36193=CARTESIAN_POINT('',(47.3400973376647,40.0183828522986,35.0304657090004));
#36194=CARTESIAN_POINT('Origin',(47.3400973376647,40.0183828522986,35.0304657090004));
#36195=CARTESIAN_POINT('Origin',(47.5336239841754,40.6309603491163,35.0304657090004));
#36196=CARTESIAN_POINT('',(47.5336239841754,40.6309603491163,35.0304657090004));
#36197=CARTESIAN_POINT('Origin',(47.5336239841754,40.6309603491163,35.0304657090004));
#36198=CARTESIAN_POINT('Origin',(47.7764374396173,41.2257253265431,35.0304657090004));
#36199=CARTESIAN_POINT('',(47.7764374396173,41.2257253265431,35.0304657090004));
#36200=CARTESIAN_POINT('Origin',(47.7764374396173,41.2257253265431,35.0304657090004));
#36201=CARTESIAN_POINT('Origin',(48.0669218205059,41.7987197217834,35.0304657090004));
#36202=CARTESIAN_POINT('',(48.0669218205059,41.7987197217834,35.0304657090004));
#36203=CARTESIAN_POINT('Origin',(48.0669218205059,41.7987197217834,35.0304657090004));
#36204=CARTESIAN_POINT('Origin',(48.4031440012129,42.3461303516745,35.0304657090004));
#36205=CARTESIAN_POINT('',(48.4031440012129,42.3461303516745,35.0304657090004));
#36206=CARTESIAN_POINT('Origin',(48.4031440012129,42.3461303516745,35.0304657090004));
#36207=CARTESIAN_POINT('Origin',(48.7828664785984,42.8643142887907,35.0304657090004));
#36208=CARTESIAN_POINT('',(48.7828664785984,42.8643142887907,35.0304657090004));
#36209=CARTESIAN_POINT('Origin',(48.7828664785984,42.8643142887907,35.0304657090004));
#36210=CARTESIAN_POINT('Origin',(49.2035622622253,43.349823104525,35.0304657090004));
#36211=CARTESIAN_POINT('',(49.2035622622253,43.349823104525,35.0304657090004));
#36212=CARTESIAN_POINT('Origin',(49.2035622622253,43.349823104525,35.0304657090004));
#36213=CARTESIAN_POINT('Origin',(49.6624316910634,43.7994258178118,35.0304657090004));
#36214=CARTESIAN_POINT('',(49.6624316910634,43.7994258178118,35.0304657090004));
#36215=CARTESIAN_POINT('Origin',(49.6624316910634,43.7994258178118,35.0304657090004));
#36216=CARTESIAN_POINT('Origin',(50.1564210647719,44.2101303967736,35.0304657090004));
#36217=CARTESIAN_POINT('',(50.1564210647719,44.2101303967736,35.0304657090004));
#36218=CARTESIAN_POINT('Origin',(50.1564210647719,44.2101303967736,35.0304657090004));
#36219=CARTESIAN_POINT('Origin',(50.6822429655713,44.5792036701988,35.0304657090004));
#36220=CARTESIAN_POINT('',(50.6822429655713,44.5792036701988,35.0304657090004));
#36221=CARTESIAN_POINT('Origin',(50.6822429655713,44.5792036701988,35.0304657090004));
#36222=CARTESIAN_POINT('Origin',(51.2363981354663,44.9041895163455,35.0304657090004));
#36223=CARTESIAN_POINT('',(51.2363981354663,44.9041895163455,35.0304657090004));
#36224=CARTESIAN_POINT('Origin',(51.2363981354663,44.9041895163455,35.0304657090004));
#36225=CARTESIAN_POINT('Origin',(51.8151987632305,45.1829252080266,35.0304657090004));
#36226=CARTESIAN_POINT('',(51.8151987632305,45.1829252080266,35.0304657090004));
#36227=CARTESIAN_POINT('Origin',(51.8151987632305,45.1829252080266,35.0304657090004));
#36228=CARTESIAN_POINT('Origin',(52.4147930261813,45.413555805202,35.0304657090004));
#36229=CARTESIAN_POINT('',(52.4147930261813,45.413555805202,35.0304657090004));
#36230=CARTESIAN_POINT('Origin',(52.4147930261813,45.413555805202,35.0304657090004));
#36231=CARTESIAN_POINT('Origin',(53.0311907234251,45.594546499299,35.0304657090004));
#36232=CARTESIAN_POINT('',(53.0311907234251,45.594546499299,35.0304657090004));
#36233=CARTESIAN_POINT('Origin',(53.0311907234251,45.594546499299,35.0304657090004));
#36234=CARTESIAN_POINT('Origin',(53.660289829985,45.7246928271096,35.0304657090004));
#36235=CARTESIAN_POINT('',(53.660289829985,45.7246928271096,35.0304657090004));
#36236=CARTESIAN_POINT('Origin',(53.660289829985,45.7246928271096,35.0304657090004));
#36237=CARTESIAN_POINT('Origin',(43.4397894030341,37.9543320991532,41.9294657090004));
#36238=CARTESIAN_POINT('',(46.1052618504143,38.3543320991532,42.1294657090004));
#36239=CARTESIAN_POINT('',(46.1052618504143,37.5543320991532,42.1294657090004));
#36240=CARTESIAN_POINT('Origin',(43.4397894030341,37.9543320991532,42.1294657090004));
#36241=CARTESIAN_POINT('',(45.2130570344595,37.5543320991532,42.8294657090004));
#36242=CARTESIAN_POINT('Ctrl Pts',(45.2130570344595,37.5543320991532,42.8294657090004));
#36243=CARTESIAN_POINT('Ctrl Pts',(45.3272286490232,37.5543320991532,42.8294657090004));
#36244=CARTESIAN_POINT('Ctrl Pts',(45.461704750062,37.5543320991532,42.8032587413542));
#36245=CARTESIAN_POINT('Ctrl Pts',(45.6711920890012,37.5543320991532,42.717234203378));
#36246=CARTESIAN_POINT('Ctrl Pts',(45.783598159642,37.5543320991532,42.6429232657692));
#36247=CARTESIAN_POINT('Ctrl Pts',(45.9421647319298,37.5543320991532,42.4854573905017));
#36248=CARTESIAN_POINT('Ctrl Pts',(46.0166939687517,37.5543320991532,42.3748001680524));
#36249=CARTESIAN_POINT('Ctrl Pts',(46.0776692182323,37.5543320991532,42.2284287129193));
#36250=CARTESIAN_POINT('Ctrl Pts',(46.0936789385295,37.5543320991532,42.1797227805058));
#36251=CARTESIAN_POINT('Ctrl Pts',(46.1052618504143,37.5543320991532,42.1294657090004));
#36252=CARTESIAN_POINT('',(41.6665217716088,37.5543320991532,42.8294657090004));
#36253=CARTESIAN_POINT('Origin',(43.4397894030341,37.9543320991532,42.8294657090004));
#36254=CARTESIAN_POINT('',(40.7743169556539,37.5543320991532,42.1294657090004));
#36255=CARTESIAN_POINT('Ctrl Pts',(40.7743169556539,37.5543320991532,42.1294657090003));
#36256=CARTESIAN_POINT('Ctrl Pts',(40.7858998675388,37.5543320991532,42.1797227805058));
#36257=CARTESIAN_POINT('Ctrl Pts',(40.801909587836,37.5543320991532,42.2284287129193));
#36258=CARTESIAN_POINT('Ctrl Pts',(40.8628848373166,37.5543320991532,42.3748001680524));
#36259=CARTESIAN_POINT('Ctrl Pts',(40.9374140741385,37.5543320991532,42.4854573905017));
#36260=CARTESIAN_POINT('Ctrl Pts',(41.0959806464263,37.5543320991532,42.6429232657692));
#36261=CARTESIAN_POINT('Ctrl Pts',(41.2083867170671,37.5543320991532,42.717234203378));
#36262=CARTESIAN_POINT('Ctrl Pts',(41.4178740560063,37.5543320991532,42.8032587413542));
#36263=CARTESIAN_POINT('Ctrl Pts',(41.5523501570451,37.5543320991532,42.8294657090004));
#36264=CARTESIAN_POINT('Ctrl Pts',(41.6665217716088,37.5543320991532,42.8294657090004));
#36265=CARTESIAN_POINT('',(40.7444706152573,37.9543320991532,42.1294657090004));
#36266=CARTESIAN_POINT('Origin',(43.4397894030341,37.9543320991532,42.1294657090004));
#36267=CARTESIAN_POINT('',(40.7253918257139,37.9543320991532,42.0079058774732));
#36268=CARTESIAN_POINT('Origin',(41.6219670539965,37.9543320991532,41.9294657090004));
#36269=CARTESIAN_POINT('',(46.1541869803544,37.9543320991532,42.0079058774732));
#36270=CARTESIAN_POINT('Origin',(43.4397894030341,37.9543320991532,42.0079058774732));
#36271=CARTESIAN_POINT('Origin',(43.4397894030341,37.9543320991532,42.0079058774732));
#36272=CARTESIAN_POINT('',(40.7743169556539,38.3543320991532,42.1294657090004));
#36273=CARTESIAN_POINT('Origin',(43.4397894030341,37.9543320991532,42.1294657090004));
#36274=CARTESIAN_POINT('',(41.6665217716088,38.3543320991532,42.8294657090004));
#36275=CARTESIAN_POINT('Ctrl Pts',(41.6665217716088,38.3543320991532,42.8294657090004));
#36276=CARTESIAN_POINT('Ctrl Pts',(41.5523501570451,38.3543320991532,42.8294657090004));
#36277=CARTESIAN_POINT('Ctrl Pts',(41.4178740560063,38.3543320991532,42.8032587413542));
#36278=CARTESIAN_POINT('Ctrl Pts',(41.2083867170671,38.3543320991532,42.717234203378));
#36279=CARTESIAN_POINT('Ctrl Pts',(41.0959806464263,38.3543320991532,42.6429232657692));
#36280=CARTESIAN_POINT('Ctrl Pts',(40.9374140741385,38.3543320991532,42.4854573905017));
#36281=CARTESIAN_POINT('Ctrl Pts',(40.8628848373166,38.3543320991532,42.3748001680524));
#36282=CARTESIAN_POINT('Ctrl Pts',(40.801909587836,38.3543320991532,42.2284287129193));
#36283=CARTESIAN_POINT('Ctrl Pts',(40.7858998675388,38.3543320991532,42.1797227805058));
#36284=CARTESIAN_POINT('Ctrl Pts',(40.7743169556539,38.3543320991532,42.1294657090004));
#36285=CARTESIAN_POINT('',(45.2130570344595,38.3543320991532,42.8294657090004));
#36286=CARTESIAN_POINT('Origin',(43.4397894030341,37.9543320991532,42.8294657090004));
#36287=CARTESIAN_POINT('Ctrl Pts',(46.1052618504143,38.3543320991532,42.1294657090004));
#36288=CARTESIAN_POINT('Ctrl Pts',(46.0936789385295,38.3543320991532,42.1797227805058));
#36289=CARTESIAN_POINT('Ctrl Pts',(46.0776692182323,38.3543320991532,42.2284287129193));
#36290=CARTESIAN_POINT('Ctrl Pts',(46.0166939687517,38.3543320991532,42.3748001680524));
#36291=CARTESIAN_POINT('Ctrl Pts',(45.9421647319298,38.3543320991532,42.4854573905017));
#36292=CARTESIAN_POINT('Ctrl Pts',(45.783598159642,38.3543320991532,42.6429232657692));
#36293=CARTESIAN_POINT('Ctrl Pts',(45.6711920890012,38.3543320991532,42.717234203378));
#36294=CARTESIAN_POINT('Ctrl Pts',(45.461704750062,38.3543320991532,42.8032587413542));
#36295=CARTESIAN_POINT('Ctrl Pts',(45.3272286490232,38.3543320991532,42.8294657090004));
#36296=CARTESIAN_POINT('Ctrl Pts',(45.2130570344595,38.3543320991532,42.8294657090004));
#36297=CARTESIAN_POINT('Origin',(43.4397894030341,37.9543320991532,42.8294657090004));
#36298=CARTESIAN_POINT('',(46.2397894030341,37.9543320991532,41.0294657090004));
#36299=CARTESIAN_POINT('Origin',(43.4397894030341,37.9543320991532,41.0294657090004));
#36300=CARTESIAN_POINT('',(46.0823098086875,37.9543320991532,42.8294657090004));
#36301=CARTESIAN_POINT('Origin',(43.4397894030341,37.9543320991532,68.2294657090003));
#36302=CARTESIAN_POINT('',(41.9397894030341,37.9543320991532,41.0294657090004));
#36303=CARTESIAN_POINT('Origin',(43.4397894030341,37.9543320991532,41.0294657090004));
#36304=CARTESIAN_POINT('',(41.9397894030341,37.9543320991532,31.0294657090004));
#36305=CARTESIAN_POINT('',(41.9397894030341,37.9543320991532,68.2294657090003));
#36306=CARTESIAN_POINT('Origin',(43.4397894030341,37.9543320991532,31.0294657090004));
#36307=CARTESIAN_POINT('Origin',(43.4397894030341,37.9543320991532,42.8294657090004));
#36308=CARTESIAN_POINT('',(46.2397894030341,38.3543320991532,42.8294657090004));
#36309=CARTESIAN_POINT('Origin',(43.4397894030341,39.4543320991532,31.0294657090004));
#36310=CARTESIAN_POINT('Origin',(43.4397894030341,37.9543320991532,42.8294657090004));
#36311=CARTESIAN_POINT('',(40.6397894030341,37.5543320991532,42.8294657090004));
#36312=CARTESIAN_POINT('Origin',(43.4397894030341,39.4543320991532,41.0294657090004));
#36313=CARTESIAN_POINT('Origin',(46.2397894030341,38.3543320991532,42.1294657090004));
#36314=CARTESIAN_POINT('',(46.2397894030341,38.3543320991532,42.1294657090004));
#36315=CARTESIAN_POINT('Origin',(40.6397894030341,37.5543320991532,42.1294657090004));
#36316=CARTESIAN_POINT('',(40.6397894030341,37.5543320991532,42.1294657090004));
#36317=CARTESIAN_POINT('Origin',(40.6397894030341,38.3543320991532,42.1294657090004));
#36318=CARTESIAN_POINT('Origin',(16.1460502915689,27.3543320991532,35.0294657090004));
#36319=CARTESIAN_POINT('',(16.1460502915689,26.8543320991532,30.5294657090004));
#36320=CARTESIAN_POINT('Origin',(16.1460502915689,26.8543320991532,35.0294657090004));
#36321=CARTESIAN_POINT('',(16.1460502915689,27.3543320991532,31.0294657090004));
#36322=CARTESIAN_POINT('Origin',(16.1460502915689,27.3543320991532,30.5294657090004));
#36323=CARTESIAN_POINT('Origin',(16.1460502915689,27.3543320991532,35.0294657090004));
#36324=CARTESIAN_POINT('Origin',(16.1460502915689,42.4643320991532,35.0294657090004));
#36325=CARTESIAN_POINT('',(18.145143062111,42.4652393286112,35.0294657090004));
#36326=CARTESIAN_POINT('',(16.1460502915689,42.4652393286112,33.0303729384583));
#36327=CARTESIAN_POINT('Origin',(16.1460502915689,42.4652393286112,35.0294657090004));
#36328=CARTESIAN_POINT('Origin',(16.1460502915689,42.4652393286112,35.0294657090004));
#36329=CARTESIAN_POINT('',(16.1460502915689,42.8543320991532,33.4194657090004));
#36330=CARTESIAN_POINT('',(16.1460502915689,42.4643320991532,33.0294657090004));
#36331=CARTESIAN_POINT('Origin',(16.1460502915689,42.8543320991532,35.0294657090004));
#36332=CARTESIAN_POINT('Origin',(16.1460502915689,42.1927936376148,35.0294657090004));
#36333=CARTESIAN_POINT('',(16.1460502915689,41.919712697713,33.0294657090004));
#36334=CARTESIAN_POINT('',(14.1460502915689,41.919712697713,35.0294657090004));
#36335=CARTESIAN_POINT('Origin',(16.1460502915689,41.919712697713,35.0294657090004));
#36336=CARTESIAN_POINT('Origin',(16.1460502915689,41.919712697713,35.0294657090004));
#36337=CARTESIAN_POINT('',(14.5360502915689,42.1927936376148,35.0294657090004));
#36338=CARTESIAN_POINT('',(14.5360502915689,42.1927936376148,35.0294657090004));
#36339=CARTESIAN_POINT('',(17.7560502915689,42.1927936376148,35.0294657090004));
#36340=CARTESIAN_POINT('Origin',(16.1460502915689,42.1927936376148,35.0294657090004));
#36341=CARTESIAN_POINT('Origin',(16.1460502915689,42.1927936376148,35.0294657090004));
#36342=CARTESIAN_POINT('Origin',(16.1460502915689,42.4658745775166,35.0294657090004));
#36343=CARTESIAN_POINT('',(18.1460502915689,42.4658745775166,35.0294657090004));
#36344=CARTESIAN_POINT('Origin',(16.1460502915689,-2.04566790084674,35.0294657090004));
#36345=CARTESIAN_POINT('',(18.1460502915689,41.8043361159781,35.0294657090004));
#36346=CARTESIAN_POINT('',(16.1460502915689,41.8043361159781,33.0294657090004));
#36347=CARTESIAN_POINT('Origin',(16.1460502915689,41.8043361159781,35.0294657090004));
#36348=CARTESIAN_POINT('Origin',(16.1460502915689,41.8043361159781,35.0294657090004));
#36349=CARTESIAN_POINT('',(16.1460502915689,-2.04566790084674,33.0294657090004));
#36350=CARTESIAN_POINT('Origin',(16.1460502915689,41.5312551760763,35.0294657090004));
#36351=CARTESIAN_POINT('',(16.1460502915689,41.2581742361745,33.0294657090004));
#36352=CARTESIAN_POINT('',(14.1460502915689,41.2581742361745,35.0294657090004));
#36353=CARTESIAN_POINT('Origin',(16.1460502915689,41.2581742361745,35.0294657090004));
#36354=CARTESIAN_POINT('Origin',(16.1460502915689,41.2581742361745,35.0294657090004));
#36355=CARTESIAN_POINT('',(14.5360502915689,41.5312551760763,35.0294657090004));
#36356=CARTESIAN_POINT('',(14.5360502915689,41.5312551760763,35.0294657090004));
#36357=CARTESIAN_POINT('',(17.7560502915689,41.5312551760763,35.0294657090004));
#36358=CARTESIAN_POINT('Origin',(16.1460502915689,41.5312551760763,35.0294657090004));
#36359=CARTESIAN_POINT('Origin',(16.1460502915689,41.5312551760763,35.0294657090004));
#36360=CARTESIAN_POINT('Origin',(16.1460502915689,41.8043361159781,35.0294657090004));
#36361=CARTESIAN_POINT('',(18.1460502915689,41.8043361159781,35.0294657090004));
#36362=CARTESIAN_POINT('Origin',(16.1460502915689,-2.04566790084674,35.0294657090004));
#36363=CARTESIAN_POINT('',(18.1460502915689,41.1427976544396,35.0294657090004));
#36364=CARTESIAN_POINT('',(16.1460502915689,41.1427976544396,33.0294657090004));
#36365=CARTESIAN_POINT('Origin',(16.1460502915689,41.1427976544396,35.0294657090004));
#36366=CARTESIAN_POINT('Origin',(16.1460502915689,41.1427976544396,35.0294657090004));
#36367=CARTESIAN_POINT('',(16.1460502915689,-2.04566790084674,33.0294657090004));
#36368=CARTESIAN_POINT('Origin',(16.1460502915689,40.8697167145378,35.0294657090004));
#36369=CARTESIAN_POINT('',(16.1460502915689,40.5966357746361,33.0294657090004));
#36370=CARTESIAN_POINT('',(14.1460502915689,40.5966357746361,35.0294657090004));
#36371=CARTESIAN_POINT('Origin',(16.1460502915689,40.5966357746361,35.0294657090004));
#36372=CARTESIAN_POINT('Origin',(16.1460502915689,40.5966357746361,35.0294657090004));
#36373=CARTESIAN_POINT('',(14.5360502915689,40.8697167145378,35.0294657090004));
#36374=CARTESIAN_POINT('',(14.5360502915689,40.8697167145378,35.0294657090004));
#36375=CARTESIAN_POINT('',(17.7560502915689,40.8697167145378,35.0294657090004));
#36376=CARTESIAN_POINT('Origin',(16.1460502915689,40.8697167145378,35.0294657090004));
#36377=CARTESIAN_POINT('Origin',(16.1460502915689,40.8697167145378,35.0294657090004));
#36378=CARTESIAN_POINT('Origin',(16.1460502915689,41.1427976544396,35.0294657090004));
#36379=CARTESIAN_POINT('',(18.1460502915689,41.1427976544396,35.0294657090004));
#36380=CARTESIAN_POINT('Origin',(16.1460502915689,-2.04566790084674,35.0294657090004));
#36381=CARTESIAN_POINT('',(18.1460502915689,40.4812591929012,35.0294657090004));
#36382=CARTESIAN_POINT('',(16.1460502915689,40.4812591929012,33.0294657090004));
#36383=CARTESIAN_POINT('Origin',(16.1460502915689,40.4812591929012,35.0294657090004));
#36384=CARTESIAN_POINT('Origin',(16.1460502915689,40.4812591929012,35.0294657090004));
#36385=CARTESIAN_POINT('',(16.1460502915689,-2.04566790084674,33.0294657090004));
#36386=CARTESIAN_POINT('Origin',(16.1460502915689,40.2081782529994,35.0294657090004));
#36387=CARTESIAN_POINT('',(16.1460502915689,39.9350973130976,33.0294657090004));
#36388=CARTESIAN_POINT('',(14.1460502915689,39.9350973130976,35.0294657090004));
#36389=CARTESIAN_POINT('Origin',(16.1460502915689,39.9350973130976,35.0294657090004));
#36390=CARTESIAN_POINT('Origin',(16.1460502915689,39.9350973130976,35.0294657090004));
#36391=CARTESIAN_POINT('',(14.5360502915689,40.2081782529994,35.0294657090004));
#36392=CARTESIAN_POINT('',(14.5360502915689,40.2081782529994,35.0294657090004));
#36393=CARTESIAN_POINT('',(17.7560502915689,40.2081782529994,35.0294657090004));
#36394=CARTESIAN_POINT('Origin',(16.1460502915689,40.2081782529994,35.0294657090004));
#36395=CARTESIAN_POINT('Origin',(16.1460502915689,40.2081782529994,35.0294657090004));
#36396=CARTESIAN_POINT('Origin',(16.1460502915689,40.4812591929012,35.0294657090004));
#36397=CARTESIAN_POINT('',(18.1460502915689,40.4812591929012,35.0294657090004));
#36398=CARTESIAN_POINT('Origin',(16.1460502915689,-2.04566790084674,35.0294657090004));
#36399=CARTESIAN_POINT('',(18.1460502915689,39.8197207313627,35.0294657090004));
#36400=CARTESIAN_POINT('',(16.1460502915689,39.8197207313627,33.0294657090004));
#36401=CARTESIAN_POINT('Origin',(16.1460502915689,39.8197207313627,35.0294657090004));
#36402=CARTESIAN_POINT('Origin',(16.1460502915689,39.8197207313627,35.0294657090004));
#36403=CARTESIAN_POINT('',(16.1460502915689,-2.04566790084674,33.0294657090004));
#36404=CARTESIAN_POINT('Origin',(16.1460502915689,39.5466397914609,35.0294657090004));
#36405=CARTESIAN_POINT('',(16.1460502915689,39.2735588515591,33.0294657090004));
#36406=CARTESIAN_POINT('',(14.1460502915689,39.2735588515591,35.0294657090004));
#36407=CARTESIAN_POINT('Origin',(16.1460502915689,39.2735588515591,35.0294657090004));
#36408=CARTESIAN_POINT('Origin',(16.1460502915689,39.2735588515591,35.0294657090004));
#36409=CARTESIAN_POINT('',(14.5360502915689,39.5466397914609,35.0294657090004));
#36410=CARTESIAN_POINT('',(14.5360502915689,39.5466397914609,35.0294657090004));
#36411=CARTESIAN_POINT('',(17.7560502915689,39.5466397914609,35.0294657090004));
#36412=CARTESIAN_POINT('Origin',(16.1460502915689,39.5466397914609,35.0294657090004));
#36413=CARTESIAN_POINT('Origin',(16.1460502915689,39.5466397914609,35.0294657090004));
#36414=CARTESIAN_POINT('Origin',(16.1460502915689,39.8197207313627,35.0294657090004));
#36415=CARTESIAN_POINT('',(18.1460502915689,39.8197207313627,35.0294657090004));
#36416=CARTESIAN_POINT('Origin',(16.1460502915689,-2.04566790084674,35.0294657090004));
#36417=CARTESIAN_POINT('',(18.1460502915689,39.1581822698242,35.0294657090004));
#36418=CARTESIAN_POINT('',(16.1460502915689,39.1581822698242,33.0294657090004));
#36419=CARTESIAN_POINT('Origin',(16.1460502915689,39.1581822698242,35.0294657090004));
#36420=CARTESIAN_POINT('Origin',(16.1460502915689,39.1581822698242,35.0294657090004));
#36421=CARTESIAN_POINT('',(16.1460502915689,-2.04566790084674,33.0294657090004));
#36422=CARTESIAN_POINT('Origin',(16.1460502915689,38.8851013299225,35.0294657090004));
#36423=CARTESIAN_POINT('',(16.1460502915689,38.6120203900207,33.0294657090004));
#36424=CARTESIAN_POINT('',(14.1460502915689,38.6120203900207,35.0294657090004));
#36425=CARTESIAN_POINT('Origin',(16.1460502915689,38.6120203900207,35.0294657090004));
#36426=CARTESIAN_POINT('Origin',(16.1460502915689,38.6120203900207,35.0294657090004));
#36427=CARTESIAN_POINT('',(14.5360502915689,38.8851013299225,35.0294657090004));
#36428=CARTESIAN_POINT('',(14.5360502915689,38.8851013299225,35.0294657090004));
#36429=CARTESIAN_POINT('',(17.7560502915689,38.8851013299225,35.0294657090004));
#36430=CARTESIAN_POINT('Origin',(16.1460502915689,38.8851013299225,35.0294657090004));
#36431=CARTESIAN_POINT('Origin',(16.1460502915689,38.8851013299225,35.0294657090004));
#36432=CARTESIAN_POINT('Origin',(16.1460502915689,39.1581822698242,35.0294657090004));
#36433=CARTESIAN_POINT('',(18.1460502915689,39.1581822698242,35.0294657090004));
#36434=CARTESIAN_POINT('Origin',(16.1460502915689,-2.04566790084674,35.0294657090004));
#36435=CARTESIAN_POINT('',(18.1460502915689,38.4966438082858,35.0294657090004));
#36436=CARTESIAN_POINT('',(16.1460502915689,38.4966438082858,33.0294657090004));
#36437=CARTESIAN_POINT('Origin',(16.1460502915689,38.4966438082858,35.0294657090004));
#36438=CARTESIAN_POINT('Origin',(16.1460502915689,38.4966438082858,35.0294657090004));
#36439=CARTESIAN_POINT('',(16.1460502915689,-2.04566790084674,33.0294657090004));
#36440=CARTESIAN_POINT('Origin',(16.1460502915689,38.223562868384,35.0294657090004));
#36441=CARTESIAN_POINT('',(16.1460502915689,37.9504819284822,33.0294657090004));
#36442=CARTESIAN_POINT('',(14.1460502915689,37.9504819284822,35.0294657090004));
#36443=CARTESIAN_POINT('Origin',(16.1460502915689,37.9504819284822,35.0294657090004));
#36444=CARTESIAN_POINT('Origin',(16.1460502915689,37.9504819284822,35.0294657090004));
#36445=CARTESIAN_POINT('',(14.5360502915689,38.223562868384,35.0294657090004));
#36446=CARTESIAN_POINT('',(14.5360502915689,38.223562868384,35.0294657090004));
#36447=CARTESIAN_POINT('',(17.7560502915689,38.223562868384,35.0294657090004));
#36448=CARTESIAN_POINT('Origin',(16.1460502915689,38.223562868384,35.0294657090004));
#36449=CARTESIAN_POINT('Origin',(16.1460502915689,38.223562868384,35.0294657090004));
#36450=CARTESIAN_POINT('Origin',(16.1460502915689,38.4966438082858,35.0294657090004));
#36451=CARTESIAN_POINT('',(18.1460502915689,38.4966438082858,35.0294657090004));
#36452=CARTESIAN_POINT('Origin',(16.1460502915689,-2.04566790084674,35.0294657090004));
#36453=CARTESIAN_POINT('',(18.1460502915689,37.8351053467473,35.0294657090004));
#36454=CARTESIAN_POINT('',(16.1460502915689,37.8351053467473,33.0294657090004));
#36455=CARTESIAN_POINT('Origin',(16.1460502915689,37.8351053467473,35.0294657090004));
#36456=CARTESIAN_POINT('Origin',(16.1460502915689,37.8351053467473,35.0294657090004));
#36457=CARTESIAN_POINT('',(16.1460502915689,-2.04566790084674,33.0294657090004));
#36458=CARTESIAN_POINT('Origin',(16.1460502915689,37.5620244068455,35.0294657090004));
#36459=CARTESIAN_POINT('',(16.1460502915689,37.2889434669437,33.0294657090004));
#36460=CARTESIAN_POINT('',(14.1460502915689,37.2889434669437,35.0294657090004));
#36461=CARTESIAN_POINT('Origin',(16.1460502915689,37.2889434669437,35.0294657090004));
#36462=CARTESIAN_POINT('Origin',(16.1460502915689,37.2889434669437,35.0294657090004));
#36463=CARTESIAN_POINT('',(14.5360502915689,37.5620244068455,35.0294657090004));
#36464=CARTESIAN_POINT('',(14.5360502915689,37.5620244068455,35.0294657090004));
#36465=CARTESIAN_POINT('',(17.7560502915689,37.5620244068455,35.0294657090004));
#36466=CARTESIAN_POINT('Origin',(16.1460502915689,37.5620244068455,35.0294657090004));
#36467=CARTESIAN_POINT('Origin',(16.1460502915689,37.5620244068455,35.0294657090004));
#36468=CARTESIAN_POINT('Origin',(16.1460502915689,37.8351053467473,35.0294657090004));
#36469=CARTESIAN_POINT('',(18.1460502915689,37.8351053467473,35.0294657090004));
#36470=CARTESIAN_POINT('Origin',(16.1460502915689,-2.04566790084674,35.0294657090004));
#36471=CARTESIAN_POINT('',(18.1460502915689,37.1735668852089,35.0294657090004));
#36472=CARTESIAN_POINT('',(16.1460502915689,37.1735668852089,33.0294657090004));
#36473=CARTESIAN_POINT('Origin',(16.1460502915689,37.1735668852089,35.0294657090004));
#36474=CARTESIAN_POINT('Origin',(16.1460502915689,37.1735668852089,35.0294657090004));
#36475=CARTESIAN_POINT('',(16.1460502915689,-2.04566790084674,33.0294657090004));
#36476=CARTESIAN_POINT('Origin',(16.1460502915689,36.9004859453071,35.0294657090004));
#36477=CARTESIAN_POINT('',(16.1460502915689,36.6274050054053,33.0294657090004));
#36478=CARTESIAN_POINT('',(14.1460502915689,36.6274050054053,35.0294657090004));
#36479=CARTESIAN_POINT('Origin',(16.1460502915689,36.6274050054053,35.0294657090004));
#36480=CARTESIAN_POINT('Origin',(16.1460502915689,36.6274050054053,35.0294657090004));
#36481=CARTESIAN_POINT('',(14.5360502915689,36.9004859453071,35.0294657090004));
#36482=CARTESIAN_POINT('',(14.5360502915689,36.9004859453071,35.0294657090004));
#36483=CARTESIAN_POINT('',(17.7560502915689,36.9004859453071,35.0294657090004));
#36484=CARTESIAN_POINT('Origin',(16.1460502915689,36.9004859453071,35.0294657090004));
#36485=CARTESIAN_POINT('Origin',(16.1460502915689,36.9004859453071,35.0294657090004));
#36486=CARTESIAN_POINT('Origin',(16.1460502915689,37.1735668852089,35.0294657090004));
#36487=CARTESIAN_POINT('',(18.1460502915689,37.1735668852089,35.0294657090004));
#36488=CARTESIAN_POINT('Origin',(16.1460502915689,-2.04566790084674,35.0294657090004));
#36489=CARTESIAN_POINT('',(18.1460502915689,36.5120284236704,35.0294657090004));
#36490=CARTESIAN_POINT('',(16.1460502915689,36.5120284236704,33.0294657090004));
#36491=CARTESIAN_POINT('Origin',(16.1460502915689,36.5120284236704,35.0294657090004));
#36492=CARTESIAN_POINT('Origin',(16.1460502915689,36.5120284236704,35.0294657090004));
#36493=CARTESIAN_POINT('',(16.1460502915689,-2.04566790084674,33.0294657090004));
#36494=CARTESIAN_POINT('Origin',(16.1460502915689,36.2389474837686,35.0294657090004));
#36495=CARTESIAN_POINT('',(16.1460502915689,35.9658665438668,33.0294657090004));
#36496=CARTESIAN_POINT('',(14.1460502915689,35.9658665438668,35.0294657090004));
#36497=CARTESIAN_POINT('Origin',(16.1460502915689,35.9658665438668,35.0294657090004));
#36498=CARTESIAN_POINT('Origin',(16.1460502915689,35.9658665438668,35.0294657090004));
#36499=CARTESIAN_POINT('',(14.5360502915689,36.2389474837686,35.0294657090004));
#36500=CARTESIAN_POINT('',(14.5360502915689,36.2389474837686,35.0294657090004));
#36501=CARTESIAN_POINT('',(17.7560502915689,36.2389474837686,35.0294657090004));
#36502=CARTESIAN_POINT('Origin',(16.1460502915689,36.2389474837686,35.0294657090004));
#36503=CARTESIAN_POINT('Origin',(16.1460502915689,36.2389474837686,35.0294657090004));
#36504=CARTESIAN_POINT('Origin',(16.1460502915689,36.5120284236704,35.0294657090004));
#36505=CARTESIAN_POINT('',(18.1460502915689,36.5120284236704,35.0294657090004));
#36506=CARTESIAN_POINT('Origin',(16.1460502915689,-2.04566790084674,35.0294657090004));
#36507=CARTESIAN_POINT('',(18.1460502915689,35.8504899621319,35.0294657090004));
#36508=CARTESIAN_POINT('',(16.1460502915689,35.8504899621319,33.0294657090004));
#36509=CARTESIAN_POINT('Origin',(16.1460502915689,35.8504899621319,35.0294657090004));
#36510=CARTESIAN_POINT('Origin',(16.1460502915689,35.8504899621319,35.0294657090004));
#36511=CARTESIAN_POINT('',(16.1460502915689,-2.04566790084674,33.0294657090004));
#36512=CARTESIAN_POINT('Origin',(16.1460502915689,35.5774090222301,35.0294657090004));
#36513=CARTESIAN_POINT('',(16.1460502915689,35.3043280823284,33.0294657090004));
#36514=CARTESIAN_POINT('',(14.1460502915689,35.3043280823284,35.0294657090004));
#36515=CARTESIAN_POINT('Origin',(16.1460502915689,35.3043280823284,35.0294657090004));
#36516=CARTESIAN_POINT('Origin',(16.1460502915689,35.3043280823284,35.0294657090004));
#36517=CARTESIAN_POINT('',(14.5360502915689,35.5774090222301,35.0294657090004));
#36518=CARTESIAN_POINT('',(14.5360502915689,35.5774090222301,35.0294657090004));
#36519=CARTESIAN_POINT('',(17.7560502915689,35.5774090222301,35.0294657090004));
#36520=CARTESIAN_POINT('Origin',(16.1460502915689,35.5774090222301,35.0294657090004));
#36521=CARTESIAN_POINT('Origin',(16.1460502915689,35.5774090222301,35.0294657090004));
#36522=CARTESIAN_POINT('Origin',(16.1460502915689,35.8504899621319,35.0294657090004));
#36523=CARTESIAN_POINT('',(18.1460502915689,35.8504899621319,35.0294657090004));
#36524=CARTESIAN_POINT('Origin',(16.1460502915689,-2.04566790084674,35.0294657090004));
#36525=CARTESIAN_POINT('',(18.1460502915689,35.1889515005935,35.0294657090004));
#36526=CARTESIAN_POINT('',(16.1460502915689,35.1889515005935,33.0294657090004));
#36527=CARTESIAN_POINT('Origin',(16.1460502915689,35.1889515005935,35.0294657090004));
#36528=CARTESIAN_POINT('Origin',(16.1460502915689,35.1889515005935,35.0294657090004));
#36529=CARTESIAN_POINT('',(16.1460502915689,-2.04566790084674,33.0294657090004));
#36530=CARTESIAN_POINT('Origin',(16.1460502915689,34.9158705606917,35.0294657090004));
#36531=CARTESIAN_POINT('',(16.1460502915689,34.6427896207899,33.0294657090004));
#36532=CARTESIAN_POINT('',(14.1460502915689,34.6427896207899,35.0294657090004));
#36533=CARTESIAN_POINT('Origin',(16.1460502915689,34.6427896207899,35.0294657090004));
#36534=CARTESIAN_POINT('Origin',(16.1460502915689,34.6427896207899,35.0294657090004));
#36535=CARTESIAN_POINT('',(14.5360502915689,34.9158705606917,35.0294657090004));
#36536=CARTESIAN_POINT('',(14.5360502915689,34.9158705606917,35.0294657090004));
#36537=CARTESIAN_POINT('',(17.7560502915689,34.9158705606917,35.0294657090004));
#36538=CARTESIAN_POINT('Origin',(16.1460502915689,34.9158705606917,35.0294657090004));
#36539=CARTESIAN_POINT('Origin',(16.1460502915689,34.9158705606917,35.0294657090004));
#36540=CARTESIAN_POINT('Origin',(16.1460502915689,35.1889515005935,35.0294657090004));
#36541=CARTESIAN_POINT('',(18.1460502915689,35.1889515005935,35.0294657090004));
#36542=CARTESIAN_POINT('Origin',(16.1460502915689,-2.04566790084674,35.0294657090004));
#36543=CARTESIAN_POINT('',(18.1460502915689,34.527413039055,35.0294657090004));
#36544=CARTESIAN_POINT('',(16.1460502915689,34.527413039055,33.0294657090004));
#36545=CARTESIAN_POINT('Origin',(16.1460502915689,34.527413039055,35.0294657090004));
#36546=CARTESIAN_POINT('Origin',(16.1460502915689,34.527413039055,35.0294657090004));
#36547=CARTESIAN_POINT('',(16.1460502915689,-2.04566790084674,33.0294657090004));
#36548=CARTESIAN_POINT('Origin',(16.1460502915689,34.2543320991532,35.0294657090004));
#36549=CARTESIAN_POINT('',(16.1460502915689,33.9812511592514,33.0294657090004));
#36550=CARTESIAN_POINT('',(14.1460502915689,33.9812511592514,35.0294657090004));
#36551=CARTESIAN_POINT('Origin',(16.1460502915689,33.9812511592514,35.0294657090004));
#36552=CARTESIAN_POINT('Origin',(16.1460502915689,33.9812511592514,35.0294657090004));
#36553=CARTESIAN_POINT('',(14.5360502915689,34.2543320991532,35.0294657090004));
#36554=CARTESIAN_POINT('',(14.5360502915689,34.2543320991532,35.0294657090004));
#36555=CARTESIAN_POINT('',(17.7560502915689,34.2543320991532,35.0294657090004));
#36556=CARTESIAN_POINT('Origin',(16.1460502915689,34.2543320991532,35.0294657090004));
#36557=CARTESIAN_POINT('Origin',(16.1460502915689,34.2543320991532,35.0294657090004));
#36558=CARTESIAN_POINT('Origin',(16.1460502915689,34.527413039055,35.0294657090004));
#36559=CARTESIAN_POINT('',(18.1460502915689,34.527413039055,35.0294657090004));
#36560=CARTESIAN_POINT('Origin',(16.1460502915689,-2.04566790084674,35.0294657090004));
#36561=CARTESIAN_POINT('',(16.1460502915689,32.8543320991532,31.0294657090004));
#36562=CARTESIAN_POINT('',(16.1460502915689,-2.04566790084674,31.0294657090004));
#36563=CARTESIAN_POINT('Origin',(16.1460502915689,32.8543320991532,35.0294657090004));
#36564=CARTESIAN_POINT('Origin',(16.1460502915689,26.4543320991532,35.0294657090004));
#36565=CARTESIAN_POINT('',(15.9854118096116,26.7543320991532,42.9028271434904));
#36566=CARTESIAN_POINT('',(16.151451780189,26.4543320991532,43.2044639245305));
#36567=CARTESIAN_POINT('Ctrl Pts',(16.151451780189,26.4543320991532,43.2044639245305));
#36568=CARTESIAN_POINT('Ctrl Pts',(16.0668800194744,26.6080253707889,43.0508264986736));
#36569=CARTESIAN_POINT('Ctrl Pts',(15.9854118096116,26.7543320991532,42.9028271434904));
#36570=CARTESIAN_POINT('',(16.4740999163387,26.4543320991532,43.1978810047409));
#36571=CARTESIAN_POINT('Origin',(16.1460502915689,26.4543320991532,35.0294657090004));
#36572=CARTESIAN_POINT('',(16.627698370541,26.7543320991532,42.8897227103981));
#36573=CARTESIAN_POINT('Ctrl Pts',(16.4740999163387,26.4543320991532,43.1978810047409));
#36574=CARTESIAN_POINT('Ctrl Pts',(16.5523346430118,26.6080253707889,43.0409218735102));
#36575=CARTESIAN_POINT('Ctrl Pts',(16.627698370541,26.7543320991532,42.8897227103981));
#36576=CARTESIAN_POINT('',(16.8177720547276,26.4543320991532,43.1768220208907));
#36577=CARTESIAN_POINT('Ctrl Pts',(16.627698370541,26.7543320991532,42.8897227103981));
#36578=CARTESIAN_POINT('Ctrl Pts',(16.7209588230625,26.6080253707889,43.0305891945183));
#36579=CARTESIAN_POINT('Ctrl Pts',(16.8177720547276,26.4543320991532,43.1768220208907));
#36580=CARTESIAN_POINT('',(17.1388100367452,26.4543320991532,43.1439621868083));
#36581=CARTESIAN_POINT('Origin',(16.1460502915689,26.4543320991532,35.0294657090004));
#36582=CARTESIAN_POINT('',(17.2667796429711,26.7543320991532,42.8243095638127));
#36583=CARTESIAN_POINT('Ctrl Pts',(17.1388100367452,26.4543320991532,43.1439621868083));
#36584=CARTESIAN_POINT('Ctrl Pts',(17.2039908174864,26.6080253707889,42.981148467619));
#36585=CARTESIAN_POINT('Ctrl Pts',(17.2667796429711,26.7543320991532,42.8243095638127));
#36586=CARTESIAN_POINT('',(17.4796221317587,26.4543320991532,43.0949608052144));
#36587=CARTESIAN_POINT('Ctrl Pts',(17.2667796429711,26.7543320991532,42.8243095638127));
#36588=CARTESIAN_POINT('Ctrl Pts',(17.3712117052267,26.6080253707889,42.9571057336593));
#36589=CARTESIAN_POINT('Ctrl Pts',(17.4796221317587,26.4543320991532,43.0949608052144));
#36590=CARTESIAN_POINT('',(17.7969135048413,26.4543320991532,43.0360427336136));
#36591=CARTESIAN_POINT('Origin',(16.1460502915689,26.4543320991532,35.0294657090004));
#36592=CARTESIAN_POINT('',(17.8984026464749,26.7543320991532,42.7070230174322));
#36593=CARTESIAN_POINT('Ctrl Pts',(17.7969135048413,26.4543320991532,43.0360427336136));
#36594=CARTESIAN_POINT('Ctrl Pts',(17.8486065723089,26.6080253707889,42.8684579249044));
#36595=CARTESIAN_POINT('Ctrl Pts',(17.8984026464749,26.7543320991532,42.7070230174322));
#36596=CARTESIAN_POINT('',(18.1325975082171,26.4543320991532,42.9594250503859));
#36597=CARTESIAN_POINT('Ctrl Pts',(17.8984026464749,26.7543320991532,42.7070230174322));
#36598=CARTESIAN_POINT('Ctrl Pts',(18.0133113403204,26.6080253707889,42.8308651364048));
#36599=CARTESIAN_POINT('Ctrl Pts',(18.1325975082171,26.4543320991532,42.9594250503859));
#36600=CARTESIAN_POINT('',(18.4440307506264,26.4543320991532,42.8748408313122));
#36601=CARTESIAN_POINT('Origin',(16.1460502915689,26.4543320991532,35.0294657090004));
#36602=CARTESIAN_POINT('',(18.5183640341747,26.7543320991532,42.5386435938719));
#36603=CARTESIAN_POINT('Ctrl Pts',(18.4440307506264,26.4543320991532,42.8748408313122));
#36604=CARTESIAN_POINT('Ctrl Pts',(18.4818920959851,26.6080253707889,42.7036001823356));
#36605=CARTESIAN_POINT('Ctrl Pts',(18.5183640341747,26.7543320991532,42.5386435938719));
#36606=CARTESIAN_POINT('',(18.772352740706,26.4543320991532,42.7711167244916));
#36607=CARTESIAN_POINT('Ctrl Pts',(18.5183640341747,26.7543320991532,42.5386435938719));
#36608=CARTESIAN_POINT('Ctrl Pts',(18.6429846612111,26.6080253707889,42.6527075131012));
#36609=CARTESIAN_POINT('Ctrl Pts',(18.772352740706,26.4543320991532,42.7711167244916));
#36610=CARTESIAN_POINT('',(19.0758553155965,26.4543320991532,42.6614292519677));
#36611=CARTESIAN_POINT('Origin',(16.1460502915689,26.4543320991532,35.0294657090004));
#36612=CARTESIAN_POINT('',(19.1225380653216,26.7543320991532,42.3202918304149));
#36613=CARTESIAN_POINT('Ctrl Pts',(19.0758553155965,26.4543320991532,42.6614292519677));
#36614=CARTESIAN_POINT('Ctrl Pts',(19.0996329778397,26.6080253707889,42.4876723409899));
#36615=CARTESIAN_POINT('Ctrl Pts',(19.1225380653216,26.7543320991532,42.3202918304149));
#36616=CARTESIAN_POINT('',(19.3946303637053,26.4543320991532,42.5312889883718));
#36617=CARTESIAN_POINT('Ctrl Pts',(19.1225380653216,26.7543320991532,42.3202918304149));
#36618=CARTESIAN_POINT('Ctrl Pts',(19.256041295837,26.6080253707889,42.4238184733377));
#36619=CARTESIAN_POINT('Ctrl Pts',(19.3946303637053,26.4543320991532,42.5312889883718));
#36620=CARTESIAN_POINT('',(19.6881825115155,26.4543320991532,42.3972282144301));
#36621=CARTESIAN_POINT('Origin',(16.1460502915689,26.4543320991532,35.0294657090004));
#36622=CARTESIAN_POINT('',(19.7069040614201,26.7543320991532,42.0534208220216));
#36623=CARTESIAN_POINT('Ctrl Pts',(19.6881825115155,26.4543320991532,42.3972282144301));
#36624=CARTESIAN_POINT('Ctrl Pts',(19.697718254224,26.6080253707889,42.2221113650258));
#36625=CARTESIAN_POINT('Ctrl Pts',(19.7069040614201,26.7543320991532,42.0534208220216));
#36626=CARTESIAN_POINT('',(19.9952892223025,26.4543320991532,42.2415378560414));
#36627=CARTESIAN_POINT('Ctrl Pts',(19.7069040614201,26.7543320991532,42.0534208220216));
#36628=CARTESIAN_POINT('Ctrl Pts',(19.8484014534418,26.6080253707889,42.1457212359098));
#36629=CARTESIAN_POINT('Ctrl Pts',(19.9952892223025,26.4543320991532,42.2415378560414));
#36630=CARTESIAN_POINT('',(20.2769374019215,26.4543320991532,42.0839959330141));
#36631=CARTESIAN_POINT('Origin',(16.1460502915689,26.4543320991532,35.0294657090004));
#36632=CARTESIAN_POINT('',(20.2675731631798,26.7543320991532,41.7398065512221));
#36633=CARTESIAN_POINT('Ctrl Pts',(20.2769374019215,26.4543320991532,42.0839959330141));
#36634=CARTESIAN_POINT('Ctrl Pts',(20.2721677663007,26.6080253707889,41.9086845189238));
#36635=CARTESIAN_POINT('Ctrl Pts',(20.2675731631798,26.7543320991532,41.7398065512221));
#36636=CARTESIAN_POINT('',(20.5703320308954,26.4543320991532,41.9037915734806));
#36637=CARTESIAN_POINT('Ctrl Pts',(20.2675731631798,26.7543320991532,41.7398065512221));
#36638=CARTESIAN_POINT('Ctrl Pts',(20.4161230749094,26.6080253707889,41.8202664920499));
#36639=CARTESIAN_POINT('Ctrl Pts',(20.5703320308954,26.4543320991532,41.9037915734806));
#36640=CARTESIAN_POINT('',(20.8382019201565,26.4543320991532,41.7238169168728));
#36641=CARTESIAN_POINT('Origin',(16.1460502915689,26.4543320991532,35.0294657090004));
#36642=CARTESIAN_POINT('',(20.8008142102323,26.7543320991532,41.3815360692459));
#36643=CARTESIAN_POINT('Ctrl Pts',(20.8382019201565,26.4543320991532,41.7238169168728));
#36644=CARTESIAN_POINT('Ctrl Pts',(20.8191586473446,26.6080253707889,41.5494776066329));
#36645=CARTESIAN_POINT('Ctrl Pts',(20.8008142102323,26.7543320991532,41.3815360692459));
#36646=CARTESIAN_POINT('',(21.1159319744682,26.4543320991532,41.5202977864757));
#36647=CARTESIAN_POINT('Ctrl Pts',(20.8008142102323,26.7543320991532,41.3815360692459));
#36648=CARTESIAN_POINT('Ctrl Pts',(20.9554280665163,26.6080253707889,41.449620089382));
#36649=CARTESIAN_POINT('Ctrl Pts',(21.1159319744682,26.4543320991532,41.5202977864757));
#36650=CARTESIAN_POINT('',(21.3682409434537,26.4543320991532,41.3190880979334));
#36651=CARTESIAN_POINT('Origin',(16.1460502915689,26.4543320991532,35.0294657090004));
#36652=CARTESIAN_POINT('',(21.3030785713881,26.7543320991532,40.9809936070401));
#36653=CARTESIAN_POINT('Ctrl Pts',(21.3682409434537,26.4543320991532,41.3190880979334));
#36654=CARTESIAN_POINT('Ctrl Pts',(21.3350507632894,26.6080253707889,41.1468810908896));
#36655=CARTESIAN_POINT('Ctrl Pts',(21.3030785713881,26.7543320991532,40.9809936070401));
#36656=CARTESIAN_POINT('',(21.628458175414,26.4543320991532,41.0936085829071));
#36657=CARTESIAN_POINT('Ctrl Pts',(21.3030785713881,26.7543320991532,40.9809936070401));
#36658=CARTESIAN_POINT('Ctrl Pts',(21.4627274425223,26.6080253707889,41.0362486185636));
#36659=CARTESIAN_POINT('Ctrl Pts',(21.628458175414,26.4543320991532,41.0936085829071));
#36660=CARTESIAN_POINT('',(21.8635271495635,26.4543320991532,40.8725028797102));
#36661=CARTESIAN_POINT('Origin',(16.1460502915689,26.4543320991532,35.0294657090004));
#36662=CARTESIAN_POINT('',(21.7710237601915,26.7543320991532,40.5408447086059));
#36663=CARTESIAN_POINT('Ctrl Pts',(21.8635271495635,26.4543320991532,40.8725028797102));
#36664=CARTESIAN_POINT('Ctrl Pts',(21.8164109372198,26.6080253707889,40.7035741850823));
#36665=CARTESIAN_POINT('Ctrl Pts',(21.7710237601915,26.7543320991532,40.5408447086059));
#36666=CARTESIAN_POINT('',(22.1044998564265,26.4543320991532,40.6265635090257));
#36667=CARTESIAN_POINT('Ctrl Pts',(21.7710237601915,26.7543320991532,40.5408447086059));
#36668=CARTESIAN_POINT('Ctrl Pts',(21.9346452092787,26.6080253707889,40.5829029985315));
#36669=CARTESIAN_POINT('Ctrl Pts',(22.1044998564265,26.4543320991532,40.6265635090257));
#36670=CARTESIAN_POINT('',(22.3207644905006,26.4543320991532,40.3870332131493));
#36671=CARTESIAN_POINT('Origin',(16.1460502915689,26.4543320991532,35.0294657090004));
#36672=CARTESIAN_POINT('',(22.2015356786164,26.7543320991532,40.0640184922428));
#36673=CARTESIAN_POINT('Ctrl Pts',(22.3207644905005,26.4543320991532,40.3870332131493));
#36674=CARTESIAN_POINT('Ctrl Pts',(22.260035796597,26.6080253707889,40.2225070235287));
#36675=CARTESIAN_POINT('Ctrl Pts',(22.2015356786164,26.7543320991532,40.0640184922428));
#36676=CARTESIAN_POINT('',(22.5408890386598,26.4543320991532,40.1222706727414));
#36677=CARTESIAN_POINT('Ctrl Pts',(22.2015356786164,26.7543320991532,40.0640184922428));
#36678=CARTESIAN_POINT('Ctrl Pts',(22.3680408319088,26.6080253707889,40.0926001695902));
#36679=CARTESIAN_POINT('Ctrl Pts',(22.5408890386598,26.4543320991532,40.1222706727413));
#36680=CARTESIAN_POINT('',(22.7369101271999,26.4543320991532,39.8659098187846));
#36681=CARTESIAN_POINT('Origin',(16.1460502915689,26.4543320991532,35.0294657090004));
#36682=CARTESIAN_POINT('',(22.5917493408754,26.7543320991532,39.55368815775));
#36683=CARTESIAN_POINT('Ctrl Pts',(22.7369101271999,26.4543320991532,39.8659098187846));
#36684=CARTESIAN_POINT('Ctrl Pts',(22.6629730911748,26.6080253707889,39.7068810288184));
#36685=CARTESIAN_POINT('Ctrl Pts',(22.5917493408754,26.7543320991532,39.55368815775));
#36686=CARTESIAN_POINT('',(22.9347216241054,26.4543320991532,39.584086059677));
#36687=CARTESIAN_POINT('Ctrl Pts',(22.5917493408754,26.7543320991532,39.55368815775));
#36688=CARTESIAN_POINT('Ctrl Pts',(22.760030134049,26.6080253707889,39.5686030161721));
#36689=CARTESIAN_POINT('Ctrl Pts',(22.9347216241054,26.4543320991532,39.584086059677));
#36690=CARTESIAN_POINT('',(23.1091946791084,26.4543320991532,39.3126006868265));
#36691=CARTESIAN_POINT('Origin',(16.1460502915689,26.4543320991532,35.0294657090004));
#36692=CARTESIAN_POINT('',(22.9390679394267,26.7543320991532,39.0132498693049));
#36693=CARTESIAN_POINT('Ctrl Pts',(23.1091946791084,26.4543320991532,39.3126006868265));
#36694=CARTESIAN_POINT('Ctrl Pts',(23.0225413397378,26.6080253707889,39.1601276068739));
#36695=CARTESIAN_POINT('Ctrl Pts',(22.9390679394267,26.7543320991532,39.0132498693049));
#36696=CARTESIAN_POINT('',(23.2833767218849,26.4543320991532,39.0155911996383));
#36697=CARTESIAN_POINT('Ctrl Pts',(22.9390679394267,26.7543320991532,39.0132498693049));
#36698=CARTESIAN_POINT('Ctrl Pts',(23.1080044915674,26.6080253707889,39.0143986528797));
#36699=CARTESIAN_POINT('Ctrl Pts',(23.2833767218849,26.4543320991532,39.0155911996383));
#36700=CARTESIAN_POINT('',(23.4351406539558,26.4543320991532,38.7307879982584));
#36701=CARTESIAN_POINT('Origin',(16.1460502915689,26.4543320991532,35.0294657090004));
#36702=CARTESIAN_POINT('',(23.2411801263005,26.7543320991532,38.4463001545511));
#36703=CARTESIAN_POINT('Ctrl Pts',(23.4351406539558,26.4543320991532,38.7307879982584));
#36704=CARTESIAN_POINT('Ctrl Pts',(23.3363476749164,26.6080253707889,38.5858853115103));
#36705=CARTESIAN_POINT('Ctrl Pts',(23.2411801263005,26.7543320991532,38.4463001545511));
#36706=CARTESIAN_POINT('',(23.5845340898466,26.4543320991532,38.4205693321238));
#36707=CARTESIAN_POINT('Ctrl Pts',(23.2411801263005,26.7543320991532,38.4463001545511));
#36708=CARTESIAN_POINT('Ctrl Pts',(23.4096481925264,26.6080253707889,38.4336752183134));
#36709=CARTESIAN_POINT('Ctrl Pts',(23.5845340898466,26.4543320991532,38.4205693321238));
#36710=CARTESIAN_POINT('',(23.7125789350568,26.4543320991532,38.1243436205306));
#36711=CARTESIAN_POINT('Origin',(16.1460502915689,26.4543320991532,35.0294657090004));
#36712=CARTESIAN_POINT('',(23.4960753947382,26.7543320991532,37.8566119703002));
#36713=CARTESIAN_POINT('Ctrl Pts',(23.7125789350568,26.4543320991532,38.1243436205305));
#36714=CARTESIAN_POINT('Ctrl Pts',(23.6023037673244,26.6080253707889,37.9879756304599));
#36715=CARTESIAN_POINT('Ctrl Pts',(23.4960753947382,26.7543320991532,37.8566119703002));
#36716=CARTESIAN_POINT('',(23.8361895753942,26.4543320991532,37.8029802294902));
#36717=CARTESIAN_POINT('Ctrl Pts',(23.4960753947382,26.7543320991532,37.8566119703002));
#36718=CARTESIAN_POINT('Ctrl Pts',(23.6629538478638,26.6080253707889,37.8302973311177));
#36719=CARTESIAN_POINT('Ctrl Pts',(23.8361895753942,26.4543320991532,37.8029802294902));
#36720=CARTESIAN_POINT('',(23.9396632164247,26.4543320991532,37.4973033409204));
#36721=CARTESIAN_POINT('Origin',(16.1460502915689,26.4543320991532,35.0294657090004));
#36722=CARTESIAN_POINT('',(23.7020574587831,26.7543320991532,37.2481095941266));
#36723=CARTESIAN_POINT('Ctrl Pts',(23.9396632164247,26.4543320991532,37.4973033409204));
#36724=CARTESIAN_POINT('Ctrl Pts',(23.8186397230465,26.6080253707889,37.370377554002));
#36725=CARTESIAN_POINT('Ctrl Pts',(23.7020574587831,26.7543320991532,37.2481095941266));
#36726=CARTESIAN_POINT('',(24.0366684527916,26.4543320991532,37.1669338453204));
#36727=CARTESIAN_POINT('Ctrl Pts',(23.7020574587831,26.7543320991532,37.2481095941266));
#36728=CARTESIAN_POINT('Ctrl Pts',(23.8662357502359,26.6080253707889,37.2082803715815));
#36729=CARTESIAN_POINT('Ctrl Pts',(24.0366684527916,26.4543320991532,37.1669338453204));
#36730=CARTESIAN_POINT('',(24.1148822896334,26.4543320991532,36.8538400090343));
#36731=CARTESIAN_POINT('Origin',(16.1460502915689,26.4543320991532,35.0294657090004));
#36732=CARTESIAN_POINT('',(23.8577555417836,26.7543320991532,36.6248425089479));
#36733=CARTESIAN_POINT('Ctrl Pts',(24.1148822896334,26.4543320991532,36.8538400090343));
#36734=CARTESIAN_POINT('Ctrl Pts',(23.9839158619903,26.6080253707889,36.7372010954389));
#36735=CARTESIAN_POINT('Ctrl Pts',(23.8577555417836,26.7543320991532,36.6248425089479));
#36736=CARTESIAN_POINT('',(24.1846365681864,26.4543320991532,36.5166629633608));
#36737=CARTESIAN_POINT('Ctrl Pts',(23.8577555417836,26.7543320991532,36.624842508948));
#36738=CARTESIAN_POINT('Ctrl Pts',(24.0181410921214,26.6080253707889,36.5717637599449));
#36739=CARTESIAN_POINT('Ctrl Pts',(24.1846365681864,26.4543320991532,36.5166629633608));
#36740=CARTESIAN_POINT('',(24.2370701006596,26.4543320991532,36.1982357671821));
#36741=CARTESIAN_POINT('Origin',(16.1460502915689,26.4543320991532,35.0294657090004));
#36742=CARTESIAN_POINT('',(23.9621334986858,26.7543320991532,35.9909584543843));
#36743=CARTESIAN_POINT('Ctrl Pts',(24.2370701006596,26.4543320991532,36.1982357671821));
#36744=CARTESIAN_POINT('Ctrl Pts',(24.0970322987197,26.6080253707889,36.0926599396356));
#36745=CARTESIAN_POINT('Ctrl Pts',(23.9621334986858,26.7543320991532,35.9909584543843));
#36746=CARTESIAN_POINT('',(24.2791092181837,26.4543320991532,35.8564950290437));
#36747=CARTESIAN_POINT('Ctrl Pts',(23.9621334986858,26.7543320991532,35.9909584543843));
#36748=CARTESIAN_POINT('Ctrl Pts',(24.1176589685329,26.6080253707889,35.9249834092406));
#36749=CARTESIAN_POINT('Ctrl Pts',(24.2791092181837,26.4543320991532,35.8564950290437));
#36750=CARTESIAN_POINT('',(24.3054135097807,26.4543320991532,35.5348535534261));
#36751=CARTESIAN_POINT('Origin',(16.1460502915689,26.4543320991532,35.0294657090004));
#36752=CARTESIAN_POINT('',(24.0144967114075,26.7543320991532,35.3506758242353));
#36753=CARTESIAN_POINT('Ctrl Pts',(24.3054135097807,26.4543320991532,35.5348535534261));
#36754=CARTESIAN_POINT('Ctrl Pts',(24.1572362620112,26.6080253707889,35.441043401642));
#36755=CARTESIAN_POINT('Ctrl Pts',(24.0144967114075,26.7543320991532,35.3506758242353));
#36756=CARTESIAN_POINT('',(24.3194577028847,26.4543320991532,35.1908233510519));
#36757=CARTESIAN_POINT('Ctrl Pts',(24.0144967114075,26.7543320991532,35.3506758242353));
#36758=CARTESIAN_POINT('Ctrl Pts',(24.164127104422,26.6080253707889,35.2722435359911));
#36759=CARTESIAN_POINT('Ctrl Pts',(24.3194577028847,26.4543320991532,35.1908233510519));
#36760=CARTESIAN_POINT('',(24.3194577028847,26.4543320991532,34.8681080669487));
#36761=CARTESIAN_POINT('Origin',(16.1460502915689,26.4543320991532,35.0294657090004));
#36762=CARTESIAN_POINT('',(24.0144967114075,26.7543320991532,34.7082555937653));
#36763=CARTESIAN_POINT('Ctrl Pts',(24.3194577028847,26.4543320991532,34.8681080669487));
#36764=CARTESIAN_POINT('Ctrl Pts',(24.164127104422,26.6080253707889,34.7866878820095));
#36765=CARTESIAN_POINT('Ctrl Pts',(24.0144967114075,26.7543320991532,34.7082555937653));
#36766=CARTESIAN_POINT('',(24.3054135097807,26.4543320991532,34.5240778645745));
#36767=CARTESIAN_POINT('Ctrl Pts',(24.0144967114075,26.7543320991532,34.7082555937653));
#36768=CARTESIAN_POINT('Ctrl Pts',(24.1572362620112,26.6080253707889,34.6178880163586));
#36769=CARTESIAN_POINT('Ctrl Pts',(24.3054135097807,26.4543320991532,34.5240778645745));
#36770=CARTESIAN_POINT('',(24.2791092181837,26.4543320991532,34.2024363889569));
#36771=CARTESIAN_POINT('Origin',(16.1460502915689,26.4543320991532,35.0294657090004));
#36772=CARTESIAN_POINT('',(23.9621334986858,26.7543320991532,34.0679729636163));
#36773=CARTESIAN_POINT('Ctrl Pts',(24.2791092181837,26.4543320991532,34.2024363889569));
#36774=CARTESIAN_POINT('Ctrl Pts',(24.1176589685329,26.6080253707889,34.1339480087601));
#36775=CARTESIAN_POINT('Ctrl Pts',(23.9621334986858,26.7543320991532,34.0679729636163));
#36776=CARTESIAN_POINT('',(24.2370701006596,26.4543320991532,33.8606956508185));
#36777=CARTESIAN_POINT('Ctrl Pts',(23.9621334986858,26.7543320991532,34.0679729636163));
#36778=CARTESIAN_POINT('Ctrl Pts',(24.0970322987197,26.6080253707889,33.9662714783651));
#36779=CARTESIAN_POINT('Ctrl Pts',(24.2370701006596,26.4543320991532,33.8606956508185));
#36780=CARTESIAN_POINT('',(24.1846365681864,26.4543320991532,33.5422684546398));
#36781=CARTESIAN_POINT('Origin',(16.1460502915689,26.4543320991532,35.0294657090004));
#36782=CARTESIAN_POINT('',(23.8577555417836,26.7543320991532,33.4340889090527));
#36783=CARTESIAN_POINT('Ctrl Pts',(24.1846365681864,26.4543320991532,33.5422684546398));
#36784=CARTESIAN_POINT('Ctrl Pts',(24.0181410921214,26.6080253707889,33.4871676580557));
#36785=CARTESIAN_POINT('Ctrl Pts',(23.8577555417836,26.7543320991532,33.4340889090527));
#36786=CARTESIAN_POINT('',(24.1148822896334,26.4543320991532,33.2050914089663));
#36787=CARTESIAN_POINT('Ctrl Pts',(23.8577555417836,26.7543320991532,33.4340889090527));
#36788=CARTESIAN_POINT('Ctrl Pts',(23.9839158619903,26.6080253707889,33.3217303225617));
#36789=CARTESIAN_POINT('Ctrl Pts',(24.1148822896333,26.4543320991532,33.2050914089663));
#36790=CARTESIAN_POINT('',(24.0366684527916,26.4543320991532,32.8919975726802));
#36791=CARTESIAN_POINT('Origin',(16.1460502915689,26.4543320991532,35.0294657090004));
#36792=CARTESIAN_POINT('',(23.7020574587831,26.7543320991532,32.8108218238741));
#36793=CARTESIAN_POINT('Ctrl Pts',(24.0366684527915,26.4543320991532,32.8919975726802));
#36794=CARTESIAN_POINT('Ctrl Pts',(23.8662357502358,26.6080253707889,32.8506510464192));
#36795=CARTESIAN_POINT('Ctrl Pts',(23.7020574587831,26.7543320991532,32.8108218238741));
#36796=CARTESIAN_POINT('',(23.9396632164247,26.4543320991532,32.5616280770803));
#36797=CARTESIAN_POINT('Ctrl Pts',(23.7020574587831,26.7543320991532,32.8108218238741));
#36798=CARTESIAN_POINT('Ctrl Pts',(23.8186397230465,26.6080253707889,32.6885538639986));
#36799=CARTESIAN_POINT('Ctrl Pts',(23.9396632164247,26.4543320991532,32.5616280770803));
#36800=CARTESIAN_POINT('',(23.8361895753941,26.4543320991532,32.2559511885104));
#36801=CARTESIAN_POINT('Origin',(16.1460502915689,26.4543320991532,35.0294657090004));
#36802=CARTESIAN_POINT('',(23.4960753947382,26.7543320991532,32.2023194477005));
#36803=CARTESIAN_POINT('Ctrl Pts',(23.8361895753941,26.4543320991532,32.2559511885104));
#36804=CARTESIAN_POINT('Ctrl Pts',(23.6629538478638,26.6080253707889,32.2286340868829));
#36805=CARTESIAN_POINT('Ctrl Pts',(23.4960753947382,26.7543320991532,32.2023194477005));
#36806=CARTESIAN_POINT('',(23.7125789350568,26.4543320991532,31.9345877974701));
#36807=CARTESIAN_POINT('Ctrl Pts',(23.4960753947382,26.7543320991532,32.2023194477005));
#36808=CARTESIAN_POINT('Ctrl Pts',(23.6023037673244,26.6080253707889,32.0709557875407));
#36809=CARTESIAN_POINT('Ctrl Pts',(23.7125789350568,26.4543320991532,31.9345877974701));
#36810=CARTESIAN_POINT('',(23.5845340898465,26.4543320991532,31.6383620858768));
#36811=CARTESIAN_POINT('Origin',(16.1460502915689,26.4543320991532,35.0294657090004));
#36812=CARTESIAN_POINT('',(23.2411801263005,26.7543320991532,31.6126312634495));
#36813=CARTESIAN_POINT('Ctrl Pts',(23.5845340898465,26.4543320991532,31.6383620858768));
#36814=CARTESIAN_POINT('Ctrl Pts',(23.4096481925263,26.6080253707889,31.6252561996872));
#36815=CARTESIAN_POINT('Ctrl Pts',(23.2411801263005,26.7543320991532,31.6126312634495));
#36816=CARTESIAN_POINT('',(23.4351406539558,26.4543320991532,31.3281434197422));
#36817=CARTESIAN_POINT('Ctrl Pts',(23.2411801263005,26.7543320991532,31.6126312634495));
#36818=CARTESIAN_POINT('Ctrl Pts',(23.3363476749164,26.6080253707889,31.4730461064903));
#36819=CARTESIAN_POINT('Ctrl Pts',(23.4351406539558,26.4543320991532,31.3281434197422));
#36820=CARTESIAN_POINT('',(23.2833767218848,26.4543320991532,31.0433402183623));
#36821=CARTESIAN_POINT('Origin',(16.1460502915689,26.4543320991532,35.0294657090004));
#36822=CARTESIAN_POINT('',(22.9390679394266,26.7543320991532,31.0456815486958));
#36823=CARTESIAN_POINT('Ctrl Pts',(23.2833767218848,26.4543320991532,31.0433402183623));
#36824=CARTESIAN_POINT('Ctrl Pts',(23.1080044915673,26.6080253707889,31.044532765121));
#36825=CARTESIAN_POINT('Ctrl Pts',(22.9390679394266,26.7543320991532,31.0456815486958));
#36826=CARTESIAN_POINT('',(23.1091946791084,26.4543320991532,30.7463307311742));
#36827=CARTESIAN_POINT('Ctrl Pts',(22.9390679394266,26.7543320991532,31.0456815486958));
#36828=CARTESIAN_POINT('Ctrl Pts',(23.0225413397378,26.6080253707889,30.8988038111267));
#36829=CARTESIAN_POINT('Ctrl Pts',(23.1091946791084,26.4543320991532,30.7463307311742));
#36830=CARTESIAN_POINT('',(22.9347216241054,26.4543320991532,30.4748453583237));
#36831=CARTESIAN_POINT('Origin',(16.1460502915689,26.4543320991532,35.0294657090004));
#36832=CARTESIAN_POINT('',(22.5917493408753,26.7543320991532,30.5052432602507));
#36833=CARTESIAN_POINT('Ctrl Pts',(22.9347216241053,26.4543320991532,30.4748453583237));
#36834=CARTESIAN_POINT('Ctrl Pts',(22.7600301340489,26.6080253707889,30.4903284018285));
#36835=CARTESIAN_POINT('Ctrl Pts',(22.5917493408753,26.7543320991532,30.5052432602507));
#36836=CARTESIAN_POINT('',(22.7369101271998,26.4543320991532,30.193021599216));
#36837=CARTESIAN_POINT('Ctrl Pts',(22.5917493408753,26.7543320991532,30.5052432602507));
#36838=CARTESIAN_POINT('Ctrl Pts',(22.6629730911747,26.6080253707889,30.3520503891823));
#36839=CARTESIAN_POINT('Ctrl Pts',(22.7369101271998,26.4543320991532,30.193021599216));
#36840=CARTESIAN_POINT('',(22.5408890386598,26.4543320991532,29.9366607452593));
#36841=CARTESIAN_POINT('Origin',(16.1460502915689,26.4543320991532,35.0294657090004));
#36842=CARTESIAN_POINT('',(22.2015356786164,26.7543320991532,29.9949129257578));
#36843=CARTESIAN_POINT('Ctrl Pts',(22.5408890386598,26.4543320991532,29.9366607452593));
#36844=CARTESIAN_POINT('Ctrl Pts',(22.3680408319087,26.6080253707889,29.9663312484104));
#36845=CARTESIAN_POINT('Ctrl Pts',(22.2015356786164,26.7543320991532,29.9949129257578));
#36846=CARTESIAN_POINT('',(22.3207644905005,26.4543320991532,29.6718982048514));
#36847=CARTESIAN_POINT('Ctrl Pts',(22.2015356786164,26.7543320991532,29.9949129257579));
#36848=CARTESIAN_POINT('Ctrl Pts',(22.2600357965969,26.6080253707889,29.836424394472));
#36849=CARTESIAN_POINT('Ctrl Pts',(22.3207644905005,26.4543320991532,29.6718982048514));
#36850=CARTESIAN_POINT('',(22.1044998564264,26.4543320991532,29.4323679089749));
#36851=CARTESIAN_POINT('Origin',(16.1460502915689,26.4543320991532,35.0294657090004));
#36852=CARTESIAN_POINT('',(21.7710237601914,26.7543320991532,29.5180867093948));
#36853=CARTESIAN_POINT('Ctrl Pts',(22.1044998564264,26.4543320991532,29.4323679089749));
#36854=CARTESIAN_POINT('Ctrl Pts',(21.9346452092787,26.6080253707889,29.4760284194691));
#36855=CARTESIAN_POINT('Ctrl Pts',(21.7710237601914,26.7543320991532,29.5180867093948));
#36856=CARTESIAN_POINT('',(21.8635271495634,26.4543320991532,29.1864285382904));
#36857=CARTESIAN_POINT('Ctrl Pts',(21.7710237601914,26.7543320991532,29.5180867093948));
#36858=CARTESIAN_POINT('Ctrl Pts',(21.8164109372197,26.6080253707889,29.3553572329184));
#36859=CARTESIAN_POINT('Ctrl Pts',(21.8635271495634,26.4543320991532,29.1864285382904));
#36860=CARTESIAN_POINT('',(21.6284581754139,26.4543320991532,28.9653228350936));
#36861=CARTESIAN_POINT('Origin',(16.1460502915689,26.4543320991532,35.0294657090004));
#36862=CARTESIAN_POINT('',(21.303078571388,26.7543320991532,29.0779378109605));
#36863=CARTESIAN_POINT('Ctrl Pts',(21.6284581754139,26.4543320991532,28.9653228350936));
#36864=CARTESIAN_POINT('Ctrl Pts',(21.4627274425222,26.6080253707889,29.022682799437));
#36865=CARTESIAN_POINT('Ctrl Pts',(21.303078571388,26.7543320991532,29.0779378109605));
#36866=CARTESIAN_POINT('',(21.3682409434536,26.4543320991532,28.7398433200673));
#36867=CARTESIAN_POINT('Ctrl Pts',(21.303078571388,26.7543320991532,29.0779378109605));
#36868=CARTESIAN_POINT('Ctrl Pts',(21.3350507632894,26.6080253707889,28.912050327111));
#36869=CARTESIAN_POINT('Ctrl Pts',(21.3682409434536,26.4543320991532,28.7398433200673));
#36870=CARTESIAN_POINT('',(21.1159319744681,26.4543320991532,28.538633631525));
#36871=CARTESIAN_POINT('Origin',(16.1460502915689,26.4543320991532,35.0294657090004));
#36872=CARTESIAN_POINT('',(20.8008142102322,26.7543320991532,28.6773953487548));
#36873=CARTESIAN_POINT('Ctrl Pts',(21.1159319744681,26.4543320991532,28.538633631525));
#36874=CARTESIAN_POINT('Ctrl Pts',(20.9554280665162,26.6080253707889,28.6093113286187));
#36875=CARTESIAN_POINT('Ctrl Pts',(20.8008142102322,26.7543320991532,28.6773953487548));
#36876=CARTESIAN_POINT('',(20.8382019201564,26.4543320991532,28.3351145011278));
#36877=CARTESIAN_POINT('Ctrl Pts',(20.8008142102322,26.7543320991532,28.6773953487548));
#36878=CARTESIAN_POINT('Ctrl Pts',(20.8191586473445,26.6080253707889,28.5094538113677));
#36879=CARTESIAN_POINT('Ctrl Pts',(20.8382019201564,26.4543320991532,28.3351145011279));
#36880=CARTESIAN_POINT('',(20.5703320308953,26.4543320991532,28.15513984452));
#36881=CARTESIAN_POINT('Origin',(16.1460502915689,26.4543320991532,35.0294657090004));
#36882=CARTESIAN_POINT('',(20.2675731631797,26.7543320991532,28.3191248667786));
#36883=CARTESIAN_POINT('Ctrl Pts',(20.5703320308953,26.4543320991532,28.15513984452));
#36884=CARTESIAN_POINT('Ctrl Pts',(20.4161230749093,26.6080253707889,28.2386649259508));
#36885=CARTESIAN_POINT('Ctrl Pts',(20.2675731631797,26.7543320991532,28.3191248667786));
#36886=CARTESIAN_POINT('',(20.2769374019214,26.4543320991532,27.9749354849866));
#36887=CARTESIAN_POINT('Ctrl Pts',(20.2675731631797,26.7543320991532,28.3191248667786));
#36888=CARTESIAN_POINT('Ctrl Pts',(20.2721677663006,26.6080253707889,28.1502468990769));
#36889=CARTESIAN_POINT('Ctrl Pts',(20.2769374019214,26.4543320991532,27.9749354849866));
#36890=CARTESIAN_POINT('',(19.9952892223024,26.4543320991532,27.8173935619593));
#36891=CARTESIAN_POINT('Origin',(16.1460502915689,26.4543320991532,35.0294657090004));
#36892=CARTESIAN_POINT('',(19.70690406142,26.7543320991532,28.0055105959791));
#36893=CARTESIAN_POINT('Ctrl Pts',(19.9952892223024,26.4543320991532,27.8173935619593));
#36894=CARTESIAN_POINT('Ctrl Pts',(19.8484014534417,26.6080253707889,27.9132101820909));
#36895=CARTESIAN_POINT('Ctrl Pts',(19.70690406142,26.7543320991532,28.0055105959791));
#36896=CARTESIAN_POINT('',(19.6881825115154,26.4543320991532,27.6617032035706));
#36897=CARTESIAN_POINT('Ctrl Pts',(19.70690406142,26.7543320991532,28.0055105959791));
#36898=CARTESIAN_POINT('Ctrl Pts',(19.6977182542239,26.6080253707889,27.8368200529749));
#36899=CARTESIAN_POINT('Ctrl Pts',(19.6881825115154,26.4543320991532,27.6617032035706));
#36900=CARTESIAN_POINT('',(19.3946303637052,26.4543320991532,27.5276424296289));
#36901=CARTESIAN_POINT('Origin',(16.1460502915689,26.4543320991532,35.0294657090004));
#36902=CARTESIAN_POINT('',(19.1225380653215,26.7543320991532,27.7386395875858));
#36903=CARTESIAN_POINT('Ctrl Pts',(19.3946303637052,26.4543320991532,27.5276424296289));
#36904=CARTESIAN_POINT('Ctrl Pts',(19.2560412958369,26.6080253707889,27.635112944663));
#36905=CARTESIAN_POINT('Ctrl Pts',(19.1225380653215,26.7543320991532,27.7386395875858));
#36906=CARTESIAN_POINT('',(19.0758553155964,26.4543320991532,27.397502166033));
#36907=CARTESIAN_POINT('Ctrl Pts',(19.1225380653215,26.7543320991532,27.7386395875858));
#36908=CARTESIAN_POINT('Ctrl Pts',(19.0996329778396,26.6080253707889,27.5712590770108));
#36909=CARTESIAN_POINT('Ctrl Pts',(19.0758553155964,26.4543320991532,27.397502166033));
#36910=CARTESIAN_POINT('',(18.7723527407059,26.4543320991532,27.2878146935091));
#36911=CARTESIAN_POINT('Origin',(16.1460502915689,26.4543320991532,35.0294657090004));
#36912=CARTESIAN_POINT('',(18.5183640341746,26.7543320991532,27.5202878241288));
#36913=CARTESIAN_POINT('Ctrl Pts',(18.7723527407059,26.4543320991532,27.2878146935091));
#36914=CARTESIAN_POINT('Ctrl Pts',(18.642984661211,26.6080253707889,27.4062239048995));
#36915=CARTESIAN_POINT('Ctrl Pts',(18.5183640341746,26.7543320991532,27.5202878241288));
#36916=CARTESIAN_POINT('',(18.4440307506263,26.4543320991532,27.1840905866885));
#36917=CARTESIAN_POINT('Ctrl Pts',(18.5183640341746,26.7543320991532,27.5202878241288));
#36918=CARTESIAN_POINT('Ctrl Pts',(18.481892095985,26.6080253707889,27.3553312356651));
#36919=CARTESIAN_POINT('Ctrl Pts',(18.4440307506263,26.4543320991532,27.1840905866885));
#36920=CARTESIAN_POINT('',(18.132597508217,26.4543320991532,27.0995063676148));
#36921=CARTESIAN_POINT('Origin',(16.1460502915689,26.4543320991532,35.0294657090004));
#36922=CARTESIAN_POINT('',(17.8984026464748,26.7543320991532,27.3519084005685));
#36923=CARTESIAN_POINT('Ctrl Pts',(18.132597508217,26.4543320991532,27.0995063676148));
#36924=CARTESIAN_POINT('Ctrl Pts',(18.0133113403203,26.6080253707889,27.2280662815959));
#36925=CARTESIAN_POINT('Ctrl Pts',(17.8984026464748,26.7543320991532,27.3519084005685));
#36926=CARTESIAN_POINT('',(17.7969135048412,26.4543320991532,27.0228886843871));
#36927=CARTESIAN_POINT('Ctrl Pts',(17.8984026464748,26.7543320991532,27.3519084005685));
#36928=CARTESIAN_POINT('Ctrl Pts',(17.8486065723088,26.6080253707889,27.1904734930963));
#36929=CARTESIAN_POINT('Ctrl Pts',(17.7969135048412,26.4543320991532,27.0228886843871));
#36930=CARTESIAN_POINT('',(17.4796221317586,26.4543320991532,26.9639706127863));
#36931=CARTESIAN_POINT('Origin',(16.1460502915689,26.4543320991532,35.0294657090004));
#36932=CARTESIAN_POINT('',(17.266779642971,26.7543320991532,27.234621854188));
#36933=CARTESIAN_POINT('Ctrl Pts',(17.4796221317586,26.4543320991532,26.9639706127863));
#36934=CARTESIAN_POINT('Ctrl Pts',(17.3712117052266,26.6080253707889,27.1018256843414));
#36935=CARTESIAN_POINT('Ctrl Pts',(17.266779642971,26.7543320991532,27.234621854188));
#36936=CARTESIAN_POINT('',(17.1388100367451,26.4543320991532,26.9149692311924));
#36937=CARTESIAN_POINT('Ctrl Pts',(17.266779642971,26.7543320991532,27.234621854188));
#36938=CARTESIAN_POINT('Ctrl Pts',(17.2039908174863,26.6080253707889,27.0777829503817));
#36939=CARTESIAN_POINT('Ctrl Pts',(17.1388100367451,26.4543320991532,26.9149692311924));
#36940=CARTESIAN_POINT('',(16.8177720547275,26.4543320991532,26.88210939711));
#36941=CARTESIAN_POINT('Origin',(16.1460502915689,26.4543320991532,35.0294657090004));
#36942=CARTESIAN_POINT('',(16.6276983705409,26.7543320991532,27.1692087076026));
#36943=CARTESIAN_POINT('Ctrl Pts',(16.8177720547275,26.4543320991532,26.88210939711));
#36944=CARTESIAN_POINT('Ctrl Pts',(16.7209588230623,26.6080253707889,27.0283422234824));
#36945=CARTESIAN_POINT('Ctrl Pts',(16.6276983705409,26.7543320991532,27.1692087076026));
#36946=CARTESIAN_POINT('',(16.4740999163386,26.4543320991532,26.8610504132598));
#36947=CARTESIAN_POINT('Ctrl Pts',(16.6276983705409,26.7543320991532,27.1692087076026));
#36948=CARTESIAN_POINT('Ctrl Pts',(16.5523346430117,26.6080253707889,27.0180095444905));
#36949=CARTESIAN_POINT('Ctrl Pts',(16.4740999163386,26.4543320991532,26.8610504132598));
#36950=CARTESIAN_POINT('',(16.1514517801889,26.4543320991532,26.8544674934702));
#36951=CARTESIAN_POINT('Origin',(16.1460502915689,26.4543320991532,35.0294657090004));
#36952=CARTESIAN_POINT('',(16.1460502915689,26.4641465066589,26.8642801165061));
#36953=CARTESIAN_POINT('Ctrl Pts',(16.1514517801889,26.4543320991532,26.8544674934702));
#36954=CARTESIAN_POINT('Ctrl Pts',(16.1487494137305,26.4592431420195,26.8593767518666));
#36955=CARTESIAN_POINT('Ctrl Pts',(16.1460502915689,26.4641465066589,26.8642801165061));
#36956=CARTESIAN_POINT('',(16.1460502915689,26.8543320991532,27.2544657090004));
#36957=CARTESIAN_POINT('',(16.1460502915689,26.4543320991532,26.8544657090004));
#36958=CARTESIAN_POINT('Origin',(16.1460502915689,26.8543320991532,35.0294657090004));
#36959=CARTESIAN_POINT('',(15.9854118096115,26.7543320991532,27.1561042745104));
#36960=CARTESIAN_POINT('Ctrl Pts',(16.1460502915689,26.4641465066589,26.8642801165061));
#36961=CARTESIAN_POINT('Ctrl Pts',(16.0642779822078,26.6126983046876,27.0128319145347));
#36962=CARTESIAN_POINT('Ctrl Pts',(15.9854118096115,26.7543320991532,27.1561042745104));
#36963=CARTESIAN_POINT('',(15.8072066798037,26.4543320991532,26.8614910514267));
#36964=CARTESIAN_POINT('Ctrl Pts',(15.9854118096115,26.7543320991532,27.1561042745104));
#36965=CARTESIAN_POINT('Ctrl Pts',(15.8979747132105,26.6080253707889,27.0115510575768));
#36966=CARTESIAN_POINT('Ctrl Pts',(15.8072066798037,26.4543320991532,26.8614910514267));
#36967=CARTESIAN_POINT('',(15.4850955596347,26.4543320991532,26.881228854175));
#36968=CARTESIAN_POINT('Origin',(16.1460502915689,26.4543320991532,35.0294657090004));
#36969=CARTESIAN_POINT('',(15.3441942712762,26.7543320991532,27.1953957627515));
#36970=CARTESIAN_POINT('Ctrl Pts',(15.4850955596347,26.4543320991532,26.881228854175));
#36971=CARTESIAN_POINT('Ctrl Pts',(15.4133280809848,26.6080253707889,27.0412484477957));
#36972=CARTESIAN_POINT('Ctrl Pts',(15.3441942712762,26.7543320991532,27.1953957627515));
#36973=CARTESIAN_POINT('',(15.1425683915998,26.4543320991532,26.9162882133188));
#36974=CARTESIAN_POINT('Ctrl Pts',(15.3441942712762,26.7543320991532,27.1953957627515));
#36975=CARTESIAN_POINT('Ctrl Pts',(15.2452656854537,26.6080253707889,27.0584504698055));
#36976=CARTESIAN_POINT('Ctrl Pts',(15.1425683915998,26.4543320991532,26.9162882133188));
#36977=CARTESIAN_POINT('',(14.8231378837717,26.4543320991532,26.9622153867842));
#36978=CARTESIAN_POINT('Origin',(16.1460502915689,26.4543320991532,35.0294657090004));
#36979=CARTESIAN_POINT('',(14.7083129524589,26.7543320991532,27.2868216939543));
#36980=CARTESIAN_POINT('Ctrl Pts',(14.8231378837717,26.4543320991532,26.9622153867842));
#36981=CARTESIAN_POINT('Ctrl Pts',(14.7646522879161,26.6080253707889,27.1275522441746));
#36982=CARTESIAN_POINT('Ctrl Pts',(14.7083129524589,26.7543320991532,27.2868216939543));
#36983=CARTESIAN_POINT('',(14.4846081098774,26.4543320991532,27.0250772328645));
#36984=CARTESIAN_POINT('Ctrl Pts',(14.7083129524589,26.7543320991532,27.2868216939543));
#36985=CARTESIAN_POINT('Ctrl Pts',(14.5985512306315,26.6080253707889,27.1583956733261));
#36986=CARTESIAN_POINT('Ctrl Pts',(14.4846081098774,26.4543320991532,27.0250772328645));
#36987=CARTESIAN_POINT('',(14.1699839717174,26.4543320991532,27.0968881392852));
#36988=CARTESIAN_POINT('Origin',(16.1460502915689,26.4543320991532,35.0294657090004));
#36989=CARTESIAN_POINT('',(14.0819995384234,26.7543320991532,27.4297736436309));
#36990=CARTESIAN_POINT('Ctrl Pts',(14.1699839717174,26.4543320991532,27.0968881392852));
#36991=CARTESIAN_POINT('Ctrl Pts',(14.1251694706471,26.6080253707889,27.2664419709379));
#36992=CARTESIAN_POINT('Ctrl Pts',(14.0819995384234,26.7543320991532,27.4297736436309));
#36993=CARTESIAN_POINT('',(13.8377044517554,26.4543320991532,27.1871341370879));
#36994=CARTESIAN_POINT('Ctrl Pts',(14.0819995384234,26.7543320991532,27.4297736436309));
#36995=CARTESIAN_POINT('Ctrl Pts',(13.9621351267405,26.6080253707889,27.310721549299));
#36996=CARTESIAN_POINT('Ctrl Pts',(13.8377044517554,26.4543320991532,27.1871341370879));
#36997=CARTESIAN_POINT('',(13.5299804549937,26.4543320991532,27.2843508867294));
#36998=CARTESIAN_POINT('Origin',(16.1460502915689,26.4543320991532,35.0294657090004));
#36999=CARTESIAN_POINT('',(13.4694220416057,26.7543320991532,27.6233002901416));
#37000=CARTESIAN_POINT('Ctrl Pts',(13.5299804549937,26.4543320991532,27.2843508867294));
#37001=CARTESIAN_POINT('Ctrl Pts',(13.4991352818195,26.6080253707889,27.4569933398693));
#37002=CARTESIAN_POINT('Ctrl Pts',(13.4694220416057,26.7543320991532,27.6233002901416));
#37003=CARTESIAN_POINT('',(13.2061624543472,26.4543320991532,27.4013804640286));
#37004=CARTESIAN_POINT('Ctrl Pts',(13.4694220416057,26.7543320991532,27.6233002901416));
#37005=CARTESIAN_POINT('Ctrl Pts',(13.3402526179508,26.6080253707889,27.5144143941516));
#37006=CARTESIAN_POINT('Ctrl Pts',(13.2061624543472,26.4543320991532,27.4013804640286));
#37007=CARTESIAN_POINT('',(12.9073864514113,26.4543320991532,27.5233560954618));
#37008=CARTESIAN_POINT('Origin',(16.1460502915689,26.4543320991532,35.0294657090004));
#37009=CARTESIAN_POINT('',(12.874657064179,26.7543320991532,27.8661137455836));
#37010=CARTESIAN_POINT('Ctrl Pts',(12.9073864514113,26.4543320991532,27.5233560954618));
#37011=CARTESIAN_POINT('Ctrl Pts',(12.8907158756715,26.6080253707889,27.6979382630472));
#37012=CARTESIAN_POINT('Ctrl Pts',(12.874657064179,26.7543320991532,27.8661137455836));
#37013=CARTESIAN_POINT('',(12.5941849254483,26.4543320991532,27.6663904397292));
#37014=CARTESIAN_POINT('Ctrl Pts',(12.874657064179,26.7543320991532,27.8661137455836));
#37015=CARTESIAN_POINT('Ctrl Pts',(12.7370422297551,26.6080253707889,27.7681186656083));
#37016=CARTESIAN_POINT('Ctrl Pts',(12.5941849254483,26.4543320991532,27.6663904397292));
#37017=CARTESIAN_POINT('',(12.3063452213432,26.4543320991532,27.8123132252514));
#37018=CARTESIAN_POINT('Origin',(16.1460502915689,26.4543320991532,35.0294657090004));
#37019=CARTESIAN_POINT('',(12.3016626689386,26.7543320991532,28.1565981264722));
#37020=CARTESIAN_POINT('Ctrl Pts',(12.3063452213432,26.4543320991532,27.8123132252514));
#37021=CARTESIAN_POINT('Ctrl Pts',(12.3039601829689,26.6080253707889,27.9876732917611));
#37022=CARTESIAN_POINT('Ctrl Pts',(12.3016626689386,26.7543320991532,28.1565981264722));
#37023=CARTESIAN_POINT('',(12.0058444745444,26.4543320991532,27.9804004665249));
#37024=CARTESIAN_POINT('Ctrl Pts',(12.3016626689386,26.7543320991532,28.1565981264722));
#37025=CARTESIAN_POINT('Ctrl Pts',(12.1565182277639,26.6080253707889,28.0701460036008));
#37026=CARTESIAN_POINT('Ctrl Pts',(12.0058444745444,26.4543320991532,27.9804004665249));
#37027=CARTESIAN_POINT('',(11.7308565950108,26.4543320991532,28.1492993140741));
#37028=CARTESIAN_POINT('Origin',(16.1460502915689,26.4543320991532,35.0294657090004));
#37029=CARTESIAN_POINT('',(11.7542520390476,26.7543320991532,28.4928203071792));
#37030=CARTESIAN_POINT('Ctrl Pts',(11.7308565950108,26.4543320991532,28.1492993140741));
#37031=CARTESIAN_POINT('Ctrl Pts',(11.7427729660389,26.6080253707889,28.3242702871977));
#37032=CARTESIAN_POINT('Ctrl Pts',(11.7542520390476,26.7543320991532,28.4928203071792));
#37033=CARTESIAN_POINT('',(11.4450564102669,26.4543320991532,28.3413208594953));
#37034=CARTESIAN_POINT('Ctrl Pts',(11.7542520390476,26.7543320991532,28.4928203071792));
#37035=CARTESIAN_POINT('Ctrl Pts',(11.6025439034309,26.6080253707889,28.4184864660259));
#37036=CARTESIAN_POINT('Ctrl Pts',(11.4450564102669,26.4543320991532,28.3413208594953));
#37037=CARTESIAN_POINT('',(11.1847503542732,26.4543320991532,28.5320717751074));
#37038=CARTESIAN_POINT('Origin',(16.1460502915689,26.4543320991532,35.0294657090004));
#37039=CARTESIAN_POINT('',(11.2360681019313,26.7543320991532,28.8725427845647));
#37040=CARTESIAN_POINT('Ctrl Pts',(11.1847503542732,26.4543320991532,28.5320717751074));
#37041=CARTESIAN_POINT('Ctrl Pts',(11.2108888332206,26.6080253707889,28.705489251887));
#37042=CARTESIAN_POINT('Ctrl Pts',(11.2360681019313,26.7543320991532,28.8725427845647));
#37043=CARTESIAN_POINT('',(10.9155526846601,26.4543320991532,28.746749752973));
#37044=CARTESIAN_POINT('Ctrl Pts',(11.2360681019313,26.7543320991532,28.8725427845647));
#37045=CARTESIAN_POINT('Ctrl Pts',(11.0788058644852,26.6080253707889,28.8108219045781));
#37046=CARTESIAN_POINT('Ctrl Pts',(10.9155526846601,26.4543320991532,28.746749752973));
#37047=CARTESIAN_POINT('',(10.6716607460615,26.4543320991532,28.9580833207762));
#37048=CARTESIAN_POINT('Origin',(16.1460502915689,26.4543320991532,35.0294657090004));
#37049=CARTESIAN_POINT('',(10.7505592861971,26.7543320991532,29.2932385681916));
#37050=CARTESIAN_POINT('Ctrl Pts',(10.6716607460615,26.4543320991532,28.9580833207762));
#37051=CARTESIAN_POINT('Ctrl Pts',(10.7118473856633,26.6080253707889,29.1287932365158));
#37052=CARTESIAN_POINT('Ctrl Pts',(10.7505592861971,26.7543320991532,29.2932385681916));
#37053=CARTESIAN_POINT('',(10.4208570576559,26.4543320991532,29.1939890845628));
#37054=CARTESIAN_POINT('Ctrl Pts',(10.7505592861971,26.7543320991532,29.2932385681916));
#37055=CARTESIAN_POINT('Ctrl Pts',(10.5887895011652,26.6080253707889,29.2445413916448));
#37056=CARTESIAN_POINT('Ctrl Pts',(10.4208570576559,26.4543320991532,29.1939890845628));
#37057=CARTESIAN_POINT('',(10.1950022970644,26.4543320991532,29.4244989145311));
#37058=CARTESIAN_POINT('Origin',(16.1460502915689,26.4543320991532,35.0294657090004));
#37059=CARTESIAN_POINT('',(10.3009565729102,26.7543320991532,29.7521079970296));
#37060=CARTESIAN_POINT('Ctrl Pts',(10.1950022970644,26.4543320991532,29.4244989145311));
#37061=CARTESIAN_POINT('Ctrl Pts',(10.2489696618644,26.6080253707889,29.5913652229065));
#37062=CARTESIAN_POINT('Ctrl Pts',(10.3009565729103,26.7543320991532,29.7521079970296));
#37063=CARTESIAN_POINT('',(9.96426164703304,26.4543320991532,29.6800625503025));
#37064=CARTESIAN_POINT('Ctrl Pts',(10.3009565729102,26.7543320991532,29.7521079970296));
#37065=CARTESIAN_POINT('Ctrl Pts',(10.1357557915219,26.6080253707889,29.7167585955981));
#37066=CARTESIAN_POINT('Ctrl Pts',(9.96426164703304,26.4543320991532,29.6800625503025));
#37067=CARTESIAN_POINT('',(9.75794709061692,26.4543320991532,29.9282146375487));
#37068=CARTESIAN_POINT('Origin',(16.1460502915689,26.4543320991532,35.0294657090004));
#37069=CARTESIAN_POINT('',(9.89025199394849,26.7543320991532,30.2460973707382));
#37070=CARTESIAN_POINT('Ctrl Pts',(9.75794709061692,26.4543320991532,29.9282146375487));
#37071=CARTESIAN_POINT('Ctrl Pts',(9.82533603670637,26.6080253707889,30.0901268708088));
#37072=CARTESIAN_POINT('Ctrl Pts',(9.89025199394849,26.7543320991532,30.2460973707382));
#37073=CARTESIAN_POINT('',(9.5488050199162,26.4543320991532,30.2017354114738));
#37074=CARTESIAN_POINT('Ctrl Pts',(9.89025199394848,26.7543320991532,30.2460973707382));
#37075=CARTESIAN_POINT('Ctrl Pts',(9.7227196001476,26.6080253707889,30.2243309888561));
#37076=CARTESIAN_POINT('Ctrl Pts',(9.5488050199162,26.4543320991532,30.2017354114738));
#37077=CARTESIAN_POINT('',(9.36340365700895,26.4543320991532,30.4658783447997));
#37078=CARTESIAN_POINT('Origin',(16.1460502915689,26.4543320991532,35.0294657090004));
#37079=CARTESIAN_POINT('',(9.52117872052333,26.7543320991532,30.7719192715376));
#37080=CARTESIAN_POINT('Ctrl Pts',(9.36340365700896,26.4543320991532,30.4658783447997));
#37081=CARTESIAN_POINT('Ctrl Pts',(9.44376572207002,26.6080253707889,30.6217590037456));
#37082=CARTESIAN_POINT('Ctrl Pts',(9.52117872052333,26.7543320991532,30.7719192715376));
#37083=CARTESIAN_POINT('',(9.17725197161336,26.4543320991532,30.7555360212558));
#37084=CARTESIAN_POINT('Ctrl Pts',(9.52117872052333,26.7543320991532,30.7719192715376));
#37085=CARTESIAN_POINT('Ctrl Pts',(9.35242961474975,26.6080253707889,30.7638807608853));
#37086=CARTESIAN_POINT('Ctrl Pts',(9.17725197161336,26.4543320991532,30.7555360212558));
#37087=CARTESIAN_POINT('',(9.01399761769606,26.4543320991532,31.0339119730205));
#37088=CARTESIAN_POINT('Origin',(16.1460502915689,26.4543320991532,35.0294657090004));
#37089=CARTESIAN_POINT('',(9.19619287437661,26.7543320991532,31.3260744414326));
#37090=CARTESIAN_POINT('Ctrl Pts',(9.01399761769606,26.4543320991532,31.0339119730205));
#37091=CARTESIAN_POINT('Ctrl Pts',(9.10679800544456,26.6080253707889,31.1827236975856));
#37092=CARTESIAN_POINT('Ctrl Pts',(9.19619287437661,26.7543320991532,31.3260744414327));
#37093=CARTESIAN_POINT('',(8.85207512635903,26.4543320991532,31.3377789279609));
#37094=CARTESIAN_POINT('Ctrl Pts',(9.19619287437661,26.7543320991532,31.3260744414326));
#37095=CARTESIAN_POINT('Ctrl Pts',(9.02735005408761,26.6080253707889,31.3318172969722));
#37096=CARTESIAN_POINT('Ctrl Pts',(8.85207512635903,26.4543320991532,31.3377789279609));
#37097=CARTESIAN_POINT('',(8.71205421222193,26.4543320991532,31.6285353521343));
#37098=CARTESIAN_POINT('Origin',(16.1460502915689,26.4543320991532,35.0294657090004));
#37099=CARTESIAN_POINT('',(8.91745718269554,26.7543320991532,31.9048750691968));
#37100=CARTESIAN_POINT('Ctrl Pts',(8.71205421222193,26.4543320991532,31.6285353521343));
#37101=CARTESIAN_POINT('Ctrl Pts',(8.81667535138839,26.6080253707889,31.7692878248437));
#37102=CARTESIAN_POINT('Ctrl Pts',(8.91745718269554,26.7543320991532,31.9048750691968));
#37103=CARTESIAN_POINT('',(8.57543848240798,26.4543320991532,31.9445894011085));
#37104=CARTESIAN_POINT('Ctrl Pts',(8.91745718269554,26.7543320991532,31.9048750691968));
#37105=CARTESIAN_POINT('Ctrl Pts',(8.74964426900305,26.6080253707889,31.9243610731722));
#37106=CARTESIAN_POINT('Ctrl Pts',(8.57543848240799,26.4543320991532,31.9445894011085));
#37107=CARTESIAN_POINT('',(8.45958282413283,26.4543320991532,32.245791361659));
#37108=CARTESIAN_POINT('Origin',(16.1460502915689,26.4543320991532,35.0294657090004));
#37109=CARTESIAN_POINT('',(8.68682658552011,26.7543320991532,32.5044693321477));
#37110=CARTESIAN_POINT('Ctrl Pts',(8.45958282413283,26.4543320991532,32.245791361659));
#37111=CARTESIAN_POINT('Ctrl Pts',(8.57532847829738,26.6080253707889,32.3775478980294));
#37112=CARTESIAN_POINT('Ctrl Pts',(8.68682658552011,26.7543320991532,32.5044693321477));
#37113=CARTESIAN_POINT('',(8.34918301098387,26.4543320991532,32.5719292171162));
#37114=CARTESIAN_POINT('Ctrl Pts',(8.68682658552011,26.7543320991532,32.5044693321477));
#37115=CARTESIAN_POINT('Ctrl Pts',(8.52116034567757,26.6080253707889,32.5375688084173));
#37116=CARTESIAN_POINT('Ctrl Pts',(8.34918301098388,26.4543320991532,32.5719292171162));
#37117=CARTESIAN_POINT('',(8.25826360886166,26.4543320991532,32.8815722646913));
#37118=CARTESIAN_POINT('Origin',(16.1460502915689,26.4543320991532,35.0294657090004));
#37119=CARTESIAN_POINT('',(8.50583589142315,26.7543320991532,33.1208670293914));
#37120=CARTESIAN_POINT('Ctrl Pts',(8.25826360886166,26.4543320991532,32.8815722646913));
#37121=CARTESIAN_POINT('Ctrl Pts',(8.38436350979251,26.6080253707889,33.0034560467115));
#37122=CARTESIAN_POINT('Ctrl Pts',(8.50583589142315,26.7543320991532,33.1208670293914));
#37123=CARTESIAN_POINT('',(8.17481440491951,26.4543320991532,33.2156235330125));
#37124=CARTESIAN_POINT('Ctrl Pts',(8.50583589142315,26.7543320991532,33.1208670293914));
#37125=CARTESIAN_POINT('Ctrl Pts',(8.3434188069237,26.6080253707889,33.1673597064018));
#37126=CARTESIAN_POINT('Ctrl Pts',(8.17481440491951,26.4543320991532,33.2156235330125));
#37127=CARTESIAN_POINT('',(8.1094363125707,26.4543320991532,33.5316470442181));
#37128=CARTESIAN_POINT('Origin',(16.1460502915689,26.4543320991532,35.0294657090004));
#37129=CARTESIAN_POINT('',(8.37568956361252,26.7543320991532,33.7499661359513));
#37130=CARTESIAN_POINT('Ctrl Pts',(8.10943631257071,26.4543320991532,33.5316470442181));
#37131=CARTESIAN_POINT('Ctrl Pts',(8.24505128623219,26.6080253707889,33.642846955428));
#37132=CARTESIAN_POINT('Ctrl Pts',(8.37568956361252,26.7543320991532,33.7499661359513));
#37133=CARTESIAN_POINT('',(8.05349305851944,26.4543320991532,33.8713886693271));
#37134=CARTESIAN_POINT('Ctrl Pts',(8.37568956361252,26.7543320991532,33.7499661359513));
#37135=CARTESIAN_POINT('Ctrl Pts',(8.21760249335657,26.6080253707889,33.8095426126077));
#37136=CARTESIAN_POINT('Ctrl Pts',(8.05349305851944,26.4543320991532,33.8713886693271));
#37137=CARTESIAN_POINT('',(8.01409135636201,26.4543320991532,34.1916895598362));
#37138=CARTESIAN_POINT('Origin',(16.1460502915689,26.4543320991532,35.0294657090004));
#37139=CARTESIAN_POINT('',(8.29725370442715,26.7543320991532,34.3875801010673));
#37140=CARTESIAN_POINT('Ctrl Pts',(8.01409135636201,26.4543320991532,34.1916895598362));
#37141=CARTESIAN_POINT('Ctrl Pts',(8.1583189074793,26.6080253707889,34.2914655831736));
#37142=CARTESIAN_POINT('Ctrl Pts',(8.29725370442715,26.7543320991532,34.3875801010673));
#37143=CARTESIAN_POINT('',(7.98602634532736,26.4543320991532,34.5348606172715));
#37144=CARTESIAN_POINT('Ctrl Pts',(8.29725370442715,26.7543320991532,34.3875801010674));
#37145=CARTESIAN_POINT('Ctrl Pts',(8.14454869178473,26.6080253707889,34.4598439057469));
#37146=CARTESIAN_POINT('Ctrl Pts',(7.98602634532737,26.4543320991532,34.5348606172715));
#37147=CARTESIAN_POINT('',(7.97286324518834,26.4543320991532,34.8573073375037));
#37148=CARTESIAN_POINT('Origin',(16.1460502915689,26.4543320991532,35.0294657090004));
#37149=CARTESIAN_POINT('',(8.27105029156894,26.7543320991532,35.0294657090004));
#37150=CARTESIAN_POINT('Ctrl Pts',(7.97286324518834,26.4543320991532,34.8573073375037));
#37151=CARTESIAN_POINT('Ctrl Pts',(8.12474356320462,26.6080253707889,34.944995479995));
#37152=CARTESIAN_POINT('Ctrl Pts',(8.27105029156894,26.7543320991532,35.0294657090004));
#37153=CARTESIAN_POINT('',(7.97286324518834,26.4543320991532,35.2016240804971));
#37154=CARTESIAN_POINT('Ctrl Pts',(8.27105029156894,26.7543320991532,35.0294657090004));
#37155=CARTESIAN_POINT('Ctrl Pts',(8.12474356320462,26.6080253707889,35.1139359380058));
#37156=CARTESIAN_POINT('Ctrl Pts',(7.97286324518834,26.4543320991532,35.2016240804971));
#37157=CARTESIAN_POINT('',(7.98602634532737,26.4543320991532,35.5240708007294));
#37158=CARTESIAN_POINT('Origin',(16.1460502915689,26.4543320991532,35.0294657090004));
#37159=CARTESIAN_POINT('',(8.29725370442716,26.7543320991532,35.6713513169335));
#37160=CARTESIAN_POINT('Ctrl Pts',(7.98602634532737,26.4543320991532,35.5240708007294));
#37161=CARTESIAN_POINT('Ctrl Pts',(8.14454869178474,26.6080253707889,35.5990875122539));
#37162=CARTESIAN_POINT('Ctrl Pts',(8.29725370442716,26.7543320991532,35.6713513169335));
#37163=CARTESIAN_POINT('',(8.01409135636202,26.4543320991532,35.8672418581646));
#37164=CARTESIAN_POINT('Ctrl Pts',(8.29725370442716,26.7543320991532,35.6713513169335));
#37165=CARTESIAN_POINT('Ctrl Pts',(8.15831890747931,26.6080253707889,35.7674658348273));
#37166=CARTESIAN_POINT('Ctrl Pts',(8.01409135636202,26.4543320991532,35.8672418581646));
#37167=CARTESIAN_POINT('',(8.05349305851946,26.4543320991532,36.1875427486737));
#37168=CARTESIAN_POINT('Origin',(16.1460502915689,26.4543320991532,35.0294657090004));
#37169=CARTESIAN_POINT('',(8.37568956361253,26.7543320991532,36.3089652820495));
#37170=CARTESIAN_POINT('Ctrl Pts',(8.05349305851946,26.4543320991532,36.1875427486737));
#37171=CARTESIAN_POINT('Ctrl Pts',(8.21760249335659,26.6080253707889,36.2493888053931));
#37172=CARTESIAN_POINT('Ctrl Pts',(8.37568956361253,26.7543320991532,36.3089652820495));
#37173=CARTESIAN_POINT('',(8.10943631257072,26.4543320991532,36.5272843737828));
#37174=CARTESIAN_POINT('Ctrl Pts',(8.37568956361254,26.7543320991532,36.3089652820495));
#37175=CARTESIAN_POINT('Ctrl Pts',(8.24505128623221,26.6080253707889,36.4160844625728));
#37176=CARTESIAN_POINT('Ctrl Pts',(8.10943631257073,26.4543320991532,36.5272843737828));
#37177=CARTESIAN_POINT('',(8.17481440491953,26.4543320991532,36.8433078849883));
#37178=CARTESIAN_POINT('Origin',(16.1460502915689,26.4543320991532,35.0294657090004));
#37179=CARTESIAN_POINT('',(8.50583589142318,26.7543320991532,36.9380643886094));
#37180=CARTESIAN_POINT('Ctrl Pts',(8.17481440491953,26.4543320991532,36.8433078849883));
#37181=CARTESIAN_POINT('Ctrl Pts',(8.34341880692373,26.6080253707889,36.8915717115991));
#37182=CARTESIAN_POINT('Ctrl Pts',(8.50583589142318,26.7543320991532,36.9380643886094));
#37183=CARTESIAN_POINT('',(8.25826360886169,26.4543320991532,37.1773591533095));
#37184=CARTESIAN_POINT('Ctrl Pts',(8.50583589142317,26.7543320991532,36.9380643886094));
#37185=CARTESIAN_POINT('Ctrl Pts',(8.38436350979254,26.6080253707889,37.0554753712894));
#37186=CARTESIAN_POINT('Ctrl Pts',(8.25826360886169,26.4543320991532,37.1773591533095));
#37187=CARTESIAN_POINT('',(8.34918301098391,26.4543320991532,37.4870022008846));
#37188=CARTESIAN_POINT('Origin',(16.1460502915689,26.4543320991532,35.0294657090004));
#37189=CARTESIAN_POINT('',(8.68682658552014,26.7543320991532,37.5544620858532));
#37190=CARTESIAN_POINT('Ctrl Pts',(8.34918301098391,26.4543320991532,37.4870022008846));
#37191=CARTESIAN_POINT('Ctrl Pts',(8.5211603456776,26.6080253707889,37.5213626095835));
#37192=CARTESIAN_POINT('Ctrl Pts',(8.68682658552014,26.7543320991532,37.5544620858532));
#37193=CARTESIAN_POINT('',(8.45958282413287,26.4543320991532,37.8131400563419));
#37194=CARTESIAN_POINT('Ctrl Pts',(8.68682658552014,26.7543320991532,37.5544620858532));
#37195=CARTESIAN_POINT('Ctrl Pts',(8.57532847829741,26.6080253707889,37.6813835199714));
#37196=CARTESIAN_POINT('Ctrl Pts',(8.45958282413287,26.4543320991532,37.8131400563418));
#37197=CARTESIAN_POINT('',(8.57543848240802,26.4543320991532,38.1143420168924));
#37198=CARTESIAN_POINT('Origin',(16.1460502915689,26.4543320991532,35.0294657090004));
#37199=CARTESIAN_POINT('',(8.91745718269558,26.7543320991532,38.154056348804));
#37200=CARTESIAN_POINT('Ctrl Pts',(8.57543848240803,26.4543320991532,38.1143420168924));
#37201=CARTESIAN_POINT('Ctrl Pts',(8.74964426900309,26.6080253707889,38.1345703448287));
#37202=CARTESIAN_POINT('Ctrl Pts',(8.91745718269558,26.7543320991532,38.154056348804));
#37203=CARTESIAN_POINT('',(8.71205421222197,26.4543320991532,38.4303960658666));
#37204=CARTESIAN_POINT('Ctrl Pts',(8.91745718269558,26.7543320991532,38.154056348804));
#37205=CARTESIAN_POINT('Ctrl Pts',(8.81667535138844,26.6080253707889,38.2896435931571));
#37206=CARTESIAN_POINT('Ctrl Pts',(8.71205421222198,26.4543320991532,38.4303960658666));
#37207=CARTESIAN_POINT('',(8.85207512635908,26.4543320991532,38.7211524900399));
#37208=CARTESIAN_POINT('Origin',(16.1460502915689,26.4543320991532,35.0294657090004));
#37209=CARTESIAN_POINT('',(9.19619287437666,26.7543320991532,38.7328569765682));
#37210=CARTESIAN_POINT('Ctrl Pts',(8.85207512635908,26.4543320991532,38.7211524900399));
#37211=CARTESIAN_POINT('Ctrl Pts',(9.02735005408766,26.6080253707889,38.7271141210286));
#37212=CARTESIAN_POINT('Ctrl Pts',(9.19619287437666,26.7543320991532,38.7328569765682));
#37213=CARTESIAN_POINT('',(9.01399761769611,26.4543320991532,39.0250194449803));
#37214=CARTESIAN_POINT('Ctrl Pts',(9.19619287437666,26.7543320991532,38.7328569765682));
#37215=CARTESIAN_POINT('Ctrl Pts',(9.10679800544461,26.6080253707889,38.8762077204153));
#37216=CARTESIAN_POINT('Ctrl Pts',(9.01399761769611,26.4543320991532,39.0250194449803));
#37217=CARTESIAN_POINT('',(9.17725197161342,26.4543320991532,39.303395396745));
#37218=CARTESIAN_POINT('Origin',(16.1460502915689,26.4543320991532,35.0294657090004));
#37219=CARTESIAN_POINT('',(9.52117872052339,26.7543320991532,39.2870121464632));
#37220=CARTESIAN_POINT('Ctrl Pts',(9.17725197161342,26.4543320991532,39.303395396745));
#37221=CARTESIAN_POINT('Ctrl Pts',(9.3524296147498,26.6080253707889,39.2950506571155));
#37222=CARTESIAN_POINT('Ctrl Pts',(9.52117872052339,26.7543320991532,39.2870121464632));
#37223=CARTESIAN_POINT('',(9.36340365700901,26.4543320991532,39.5930530732011));
#37224=CARTESIAN_POINT('Ctrl Pts',(9.52117872052339,26.7543320991532,39.2870121464632));
#37225=CARTESIAN_POINT('Ctrl Pts',(9.44376572207008,26.6080253707889,39.4371724142552));
#37226=CARTESIAN_POINT('Ctrl Pts',(9.36340365700902,26.4543320991532,39.5930530732011));
#37227=CARTESIAN_POINT('',(9.54880501991626,26.4543320991532,39.857196006527));
#37228=CARTESIAN_POINT('Origin',(16.1460502915689,26.4543320991532,35.0294657090004));
#37229=CARTESIAN_POINT('',(9.89025199394856,26.7543320991532,39.8128340472626));
#37230=CARTESIAN_POINT('Ctrl Pts',(9.54880501991627,26.4543320991532,39.857196006527));
#37231=CARTESIAN_POINT('Ctrl Pts',(9.72271960014766,26.6080253707889,39.8346004291447));
#37232=CARTESIAN_POINT('Ctrl Pts',(9.89025199394855,26.7543320991532,39.8128340472626));
#37233=CARTESIAN_POINT('',(9.75794709061698,26.4543320991532,40.1307167804521));
#37234=CARTESIAN_POINT('Ctrl Pts',(9.89025199394855,26.7543320991532,39.8128340472626));
#37235=CARTESIAN_POINT('Ctrl Pts',(9.82533603670642,26.6080253707889,39.968804547192));
#37236=CARTESIAN_POINT('Ctrl Pts',(9.75794709061698,26.4543320991532,40.1307167804521));
#37237=CARTESIAN_POINT('',(9.96426164703311,26.4543320991532,40.3788688676983));
#37238=CARTESIAN_POINT('Origin',(16.1460502915689,26.4543320991532,35.0294657090004));
#37239=CARTESIAN_POINT('',(10.3009565729103,26.7543320991532,40.3068234209711));
#37240=CARTESIAN_POINT('Ctrl Pts',(9.96426164703311,26.4543320991532,40.3788688676983));
#37241=CARTESIAN_POINT('Ctrl Pts',(10.135755791522,26.6080253707889,40.3421728224027));
#37242=CARTESIAN_POINT('Ctrl Pts',(10.3009565729103,26.7543320991532,40.3068234209711));
#37243=CARTESIAN_POINT('',(10.1950022970645,26.4543320991532,40.6344325034697));
#37244=CARTESIAN_POINT('Ctrl Pts',(10.3009565729103,26.7543320991532,40.3068234209712));
#37245=CARTESIAN_POINT('Ctrl Pts',(10.2489696618645,26.6080253707889,40.4675661950943));
#37246=CARTESIAN_POINT('Ctrl Pts',(10.1950022970645,26.4543320991532,40.6344325034697));
#37247=CARTESIAN_POINT('',(10.420857057656,26.4543320991532,40.864942333438));
#37248=CARTESIAN_POINT('Origin',(16.1460502915689,26.4543320991532,35.0294657090004));
#37249=CARTESIAN_POINT('',(10.7505592861972,26.7543320991532,40.7656928498092));
#37250=CARTESIAN_POINT('Ctrl Pts',(10.420857057656,26.4543320991532,40.864942333438));
#37251=CARTESIAN_POINT('Ctrl Pts',(10.5887895011653,26.6080253707889,40.8143900263561));
#37252=CARTESIAN_POINT('Ctrl Pts',(10.7505592861972,26.7543320991532,40.7656928498092));
#37253=CARTESIAN_POINT('',(10.6716607460615,26.4543320991532,41.1008480972246));
#37254=CARTESIAN_POINT('Ctrl Pts',(10.7505592861972,26.7543320991532,40.7656928498093));
#37255=CARTESIAN_POINT('Ctrl Pts',(10.7118473856633,26.6080253707889,40.930138181485));
#37256=CARTESIAN_POINT('Ctrl Pts',(10.6716607460615,26.4543320991532,41.1008480972246));
#37257=CARTESIAN_POINT('',(10.9155526846602,26.4543320991532,41.3121816650278));
#37258=CARTESIAN_POINT('Origin',(16.1460502915689,26.4543320991532,35.0294657090004));
#37259=CARTESIAN_POINT('',(11.2360681019314,26.7543320991532,41.1863886334361));
#37260=CARTESIAN_POINT('Ctrl Pts',(10.9155526846602,26.4543320991532,41.3121816650278));
#37261=CARTESIAN_POINT('Ctrl Pts',(11.0788058644853,26.6080253707889,41.2481095134227));
#37262=CARTESIAN_POINT('Ctrl Pts',(11.2360681019314,26.7543320991532,41.1863886334361));
#37263=CARTESIAN_POINT('',(11.1847503542733,26.4543320991532,41.5268596428934));
#37264=CARTESIAN_POINT('Ctrl Pts',(11.2360681019314,26.7543320991532,41.1863886334361));
#37265=CARTESIAN_POINT('Ctrl Pts',(11.2108888332207,26.6080253707889,41.3534421661138));
#37266=CARTESIAN_POINT('Ctrl Pts',(11.1847503542733,26.4543320991532,41.5268596428934));
#37267=CARTESIAN_POINT('',(11.445056410267,26.4543320991532,41.7176105585055));
#37268=CARTESIAN_POINT('Origin',(16.1460502915689,26.4543320991532,35.0294657090004));
#37269=CARTESIAN_POINT('',(11.7542520390477,26.7543320991532,41.5661111108216));
#37270=CARTESIAN_POINT('Ctrl Pts',(11.445056410267,26.4543320991532,41.7176105585055));
#37271=CARTESIAN_POINT('Ctrl Pts',(11.602543903431,26.6080253707889,41.6404449519749));
#37272=CARTESIAN_POINT('Ctrl Pts',(11.7542520390477,26.7543320991532,41.5661111108216));
#37273=CARTESIAN_POINT('',(11.7308565950109,26.4543320991532,41.9096321039267));
#37274=CARTESIAN_POINT('Ctrl Pts',(11.7542520390477,26.7543320991532,41.5661111108216));
#37275=CARTESIAN_POINT('Ctrl Pts',(11.742772966039,26.6080253707889,41.7346611308031));
#37276=CARTESIAN_POINT('Ctrl Pts',(11.7308565950109,26.4543320991532,41.9096321039267));
#37277=CARTESIAN_POINT('',(12.0058444745445,26.4543320991532,42.0785309514759));
#37278=CARTESIAN_POINT('Origin',(16.1460502915689,26.4543320991532,35.0294657090004));
#37279=CARTESIAN_POINT('',(12.3016626689387,26.7543320991532,41.9023332915286));
#37280=CARTESIAN_POINT('Ctrl Pts',(12.0058444745445,26.4543320991532,42.0785309514759));
#37281=CARTESIAN_POINT('Ctrl Pts',(12.156518227764,26.6080253707889,41.9887854144));
#37282=CARTESIAN_POINT('Ctrl Pts',(12.3016626689387,26.7543320991532,41.9023332915286));
#37283=CARTESIAN_POINT('',(12.3063452213433,26.4543320991532,42.2466181927493));
#37284=CARTESIAN_POINT('Ctrl Pts',(12.3016626689387,26.7543320991532,41.9023332915286));
#37285=CARTESIAN_POINT('Ctrl Pts',(12.303960182969,26.6080253707889,42.0712581262397));
#37286=CARTESIAN_POINT('Ctrl Pts',(12.3063452213433,26.4543320991532,42.2466181927493));
#37287=CARTESIAN_POINT('',(12.5941849254484,26.4543320991532,42.3925409782716));
#37288=CARTESIAN_POINT('Origin',(16.1460502915689,26.4543320991532,35.0294657090004));
#37289=CARTESIAN_POINT('',(12.8746570641791,26.7543320991532,42.1928176724172));
#37290=CARTESIAN_POINT('Ctrl Pts',(12.5941849254484,26.4543320991532,42.3925409782716));
#37291=CARTESIAN_POINT('Ctrl Pts',(12.7370422297551,26.6080253707889,42.2908127523925));
#37292=CARTESIAN_POINT('Ctrl Pts',(12.8746570641791,26.7543320991532,42.1928176724172));
#37293=CARTESIAN_POINT('',(12.9073864514114,26.4543320991532,42.5355753225389));
#37294=CARTESIAN_POINT('Ctrl Pts',(12.8746570641791,26.7543320991532,42.1928176724172));
#37295=CARTESIAN_POINT('Ctrl Pts',(12.8907158756716,26.6080253707889,42.3609931549536));
#37296=CARTESIAN_POINT('Ctrl Pts',(12.9073864514114,26.4543320991532,42.5355753225389));
#37297=CARTESIAN_POINT('',(13.2061624543473,26.4543320991532,42.6575509539721));
#37298=CARTESIAN_POINT('Origin',(16.1460502915689,26.4543320991532,35.0294657090004));
#37299=CARTESIAN_POINT('',(13.4694220416058,26.7543320991532,42.4356311278591));
#37300=CARTESIAN_POINT('Ctrl Pts',(13.2061624543473,26.4543320991532,42.6575509539721));
#37301=CARTESIAN_POINT('Ctrl Pts',(13.3402526179509,26.6080253707889,42.5445170238492));
#37302=CARTESIAN_POINT('Ctrl Pts',(13.4694220416058,26.7543320991532,42.4356311278591));
#37303=CARTESIAN_POINT('',(13.5299804549939,26.4543320991532,42.7745805312714));
#37304=CARTESIAN_POINT('Ctrl Pts',(13.4694220416058,26.7543320991532,42.4356311278591));
#37305=CARTESIAN_POINT('Ctrl Pts',(13.4991352818196,26.6080253707889,42.6019380781315));
#37306=CARTESIAN_POINT('Ctrl Pts',(13.5299804549939,26.4543320991532,42.7745805312714));
#37307=CARTESIAN_POINT('',(13.8377044517555,26.4543320991532,42.8717972809129));
#37308=CARTESIAN_POINT('Origin',(16.1460502915689,26.4543320991532,35.0294657090004));
#37309=CARTESIAN_POINT('',(14.0819995384235,26.7543320991532,42.6291577743698));
#37310=CARTESIAN_POINT('Ctrl Pts',(13.8377044517555,26.4543320991532,42.8717972809129));
#37311=CARTESIAN_POINT('Ctrl Pts',(13.9621351267406,26.6080253707889,42.7482098687017));
#37312=CARTESIAN_POINT('Ctrl Pts',(14.0819995384235,26.7543320991532,42.6291577743698));
#37313=CARTESIAN_POINT('',(14.1699839717175,26.4543320991532,42.9620432787156));
#37314=CARTESIAN_POINT('Ctrl Pts',(14.0819995384235,26.7543320991532,42.6291577743698));
#37315=CARTESIAN_POINT('Ctrl Pts',(14.1251694706472,26.6080253707889,42.7924894470628));
#37316=CARTESIAN_POINT('Ctrl Pts',(14.1699839717175,26.4543320991532,42.9620432787156));
#37317=CARTESIAN_POINT('',(14.4846081098775,26.4543320991532,43.0338541851362));
#37318=CARTESIAN_POINT('Origin',(16.1460502915689,26.4543320991532,35.0294657090004));
#37319=CARTESIAN_POINT('',(14.708312952459,26.7543320991532,42.7721097240465));
#37320=CARTESIAN_POINT('Ctrl Pts',(14.4846081098775,26.4543320991532,43.0338541851362));
#37321=CARTESIAN_POINT('Ctrl Pts',(14.5985512306316,26.6080253707889,42.9005357446746));
#37322=CARTESIAN_POINT('Ctrl Pts',(14.708312952459,26.7543320991532,42.7721097240465));
#37323=CARTESIAN_POINT('',(14.8231378837718,26.4543320991532,43.0967160312165));
#37324=CARTESIAN_POINT('Ctrl Pts',(14.708312952459,26.7543320991532,42.7721097240464));
#37325=CARTESIAN_POINT('Ctrl Pts',(14.7646522879162,26.6080253707889,42.9313791738261));
#37326=CARTESIAN_POINT('Ctrl Pts',(14.8231378837718,26.4543320991532,43.0967160312165));
#37327=CARTESIAN_POINT('',(15.1425683915999,26.4543320991532,43.142643204682));
#37328=CARTESIAN_POINT('Origin',(16.1460502915689,26.4543320991532,35.0294657090004));
#37329=CARTESIAN_POINT('',(15.3441942712763,26.7543320991532,42.8635356552493));
#37330=CARTESIAN_POINT('Ctrl Pts',(15.1425683915999,26.4543320991532,43.142643204682));
#37331=CARTESIAN_POINT('Ctrl Pts',(15.2452656854538,26.6080253707889,43.0004809481952));
#37332=CARTESIAN_POINT('Ctrl Pts',(15.3441942712763,26.7543320991532,42.8635356552493));
#37333=CARTESIAN_POINT('',(15.4850955596348,26.4543320991532,43.1777025638257));
#37334=CARTESIAN_POINT('Ctrl Pts',(15.3441942712763,26.7543320991532,42.8635356552493));
#37335=CARTESIAN_POINT('Ctrl Pts',(15.4133280809849,26.6080253707889,43.017682970205));
#37336=CARTESIAN_POINT('Ctrl Pts',(15.4850955596348,26.4543320991532,43.1777025638257));
#37337=CARTESIAN_POINT('',(15.8072066798038,26.4543320991532,43.197440366574));
#37338=CARTESIAN_POINT('Origin',(16.1460502915689,26.4543320991532,35.0294657090004));
#37339=CARTESIAN_POINT('Ctrl Pts',(15.8072066798038,26.4543320991532,43.197440366574));
#37340=CARTESIAN_POINT('Ctrl Pts',(15.8979747132106,26.6080253707889,43.0473803604239));
#37341=CARTESIAN_POINT('Ctrl Pts',(15.9854118096116,26.7543320991532,42.9028271434904));
#37342=CARTESIAN_POINT('Origin',(16.1460502915689,23.7543320991532,35.0294657090004));
#37343=CARTESIAN_POINT('',(16.1514517801889,23.7543320991532,26.8544674934702));
#37344=CARTESIAN_POINT('',(15.9854118096115,23.4543320991532,27.1561042745104));
#37345=CARTESIAN_POINT('Ctrl Pts',(16.1514517801889,23.7543320991532,26.8544674934702));
#37346=CARTESIAN_POINT('Ctrl Pts',(16.0668800194743,23.6006388275175,27.0081049193271));
#37347=CARTESIAN_POINT('Ctrl Pts',(15.9854118096115,23.4543320991532,27.1561042745104));
#37348=CARTESIAN_POINT('',(16.4740999163386,23.7543320991532,26.8610504132598));
#37349=CARTESIAN_POINT('Origin',(16.1460502915689,23.7543320991532,35.0294657090004));
#37350=CARTESIAN_POINT('',(16.6276983705409,23.4543320991532,27.1692087076026));
#37351=CARTESIAN_POINT('Ctrl Pts',(16.6276983705409,23.4543320991532,27.1692087076026));
#37352=CARTESIAN_POINT('Ctrl Pts',(16.5523346430117,23.6006388275175,27.0180095444905));
#37353=CARTESIAN_POINT('Ctrl Pts',(16.4740999163386,23.7543320991532,26.8610504132598));
#37354=CARTESIAN_POINT('',(16.8177720547275,23.7543320991532,26.88210939711));
#37355=CARTESIAN_POINT('Ctrl Pts',(16.8177720547275,23.7543320991532,26.88210939711));
#37356=CARTESIAN_POINT('Ctrl Pts',(16.7209588230624,23.6006388275175,27.0283422234824));
#37357=CARTESIAN_POINT('Ctrl Pts',(16.6276983705409,23.4543320991532,27.1692087076026));
#37358=CARTESIAN_POINT('',(17.1388100367451,23.7543320991532,26.9149692311924));
#37359=CARTESIAN_POINT('Origin',(16.1460502915689,23.7543320991532,35.0294657090004));
#37360=CARTESIAN_POINT('',(17.266779642971,23.4543320991532,27.234621854188));
#37361=CARTESIAN_POINT('Ctrl Pts',(17.266779642971,23.4543320991532,27.234621854188));
#37362=CARTESIAN_POINT('Ctrl Pts',(17.2039908174863,23.6006388275175,27.0777829503818));
#37363=CARTESIAN_POINT('Ctrl Pts',(17.1388100367451,23.7543320991532,26.9149692311924));
#37364=CARTESIAN_POINT('',(17.4796221317586,23.7543320991532,26.9639706127863));
#37365=CARTESIAN_POINT('Ctrl Pts',(17.4796221317586,23.7543320991532,26.9639706127863));
#37366=CARTESIAN_POINT('Ctrl Pts',(17.3712117052266,23.6006388275175,27.1018256843414));
#37367=CARTESIAN_POINT('Ctrl Pts',(17.266779642971,23.4543320991532,27.234621854188));
#37368=CARTESIAN_POINT('',(17.7969135048412,23.7543320991532,27.0228886843871));
#37369=CARTESIAN_POINT('Origin',(16.1460502915689,23.7543320991532,35.0294657090004));
#37370=CARTESIAN_POINT('',(17.8984026464748,23.4543320991532,27.3519084005685));
#37371=CARTESIAN_POINT('Ctrl Pts',(17.8984026464748,23.4543320991532,27.3519084005685));
#37372=CARTESIAN_POINT('Ctrl Pts',(17.8486065723088,23.6006388275175,27.1904734930963));
#37373=CARTESIAN_POINT('Ctrl Pts',(17.7969135048412,23.7543320991532,27.0228886843871));
#37374=CARTESIAN_POINT('',(18.132597508217,23.7543320991532,27.0995063676148));
#37375=CARTESIAN_POINT('Ctrl Pts',(18.132597508217,23.7543320991532,27.0995063676148));
#37376=CARTESIAN_POINT('Ctrl Pts',(18.0133113403203,23.6006388275175,27.2280662815959));
#37377=CARTESIAN_POINT('Ctrl Pts',(17.8984026464748,23.4543320991532,27.3519084005685));
#37378=CARTESIAN_POINT('',(18.4440307506263,23.7543320991532,27.1840905866885));
#37379=CARTESIAN_POINT('Origin',(16.1460502915689,23.7543320991532,35.0294657090004));
#37380=CARTESIAN_POINT('',(18.5183640341746,23.4543320991532,27.5202878241288));
#37381=CARTESIAN_POINT('Ctrl Pts',(18.5183640341746,23.4543320991532,27.5202878241288));
#37382=CARTESIAN_POINT('Ctrl Pts',(18.481892095985,23.6006388275175,27.3553312356651));
#37383=CARTESIAN_POINT('Ctrl Pts',(18.4440307506263,23.7543320991532,27.1840905866885));
#37384=CARTESIAN_POINT('',(18.7723527407059,23.7543320991532,27.2878146935091));
#37385=CARTESIAN_POINT('Ctrl Pts',(18.7723527407059,23.7543320991532,27.2878146935091));
#37386=CARTESIAN_POINT('Ctrl Pts',(18.642984661211,23.6006388275175,27.4062239048995));
#37387=CARTESIAN_POINT('Ctrl Pts',(18.5183640341746,23.4543320991532,27.5202878241288));
#37388=CARTESIAN_POINT('',(19.0758553155964,23.7543320991532,27.397502166033));
#37389=CARTESIAN_POINT('Origin',(16.1460502915689,23.7543320991532,35.0294657090004));
#37390=CARTESIAN_POINT('',(19.1225380653215,23.4543320991532,27.7386395875858));
#37391=CARTESIAN_POINT('Ctrl Pts',(19.1225380653215,23.4543320991532,27.7386395875858));
#37392=CARTESIAN_POINT('Ctrl Pts',(19.0996329778396,23.6006388275175,27.5712590770108));
#37393=CARTESIAN_POINT('Ctrl Pts',(19.0758553155964,23.7543320991532,27.397502166033));
#37394=CARTESIAN_POINT('',(19.3946303637052,23.7543320991532,27.5276424296289));
#37395=CARTESIAN_POINT('Ctrl Pts',(19.3946303637052,23.7543320991532,27.5276424296289));
#37396=CARTESIAN_POINT('Ctrl Pts',(19.2560412958369,23.6006388275175,27.635112944663));
#37397=CARTESIAN_POINT('Ctrl Pts',(19.1225380653215,23.4543320991532,27.7386395875858));
#37398=CARTESIAN_POINT('',(19.6881825115154,23.7543320991532,27.6617032035706));
#37399=CARTESIAN_POINT('Origin',(16.1460502915689,23.7543320991532,35.0294657090004));
#37400=CARTESIAN_POINT('',(19.70690406142,23.4543320991532,28.0055105959791));
#37401=CARTESIAN_POINT('Ctrl Pts',(19.70690406142,23.4543320991532,28.0055105959791));
#37402=CARTESIAN_POINT('Ctrl Pts',(19.6977182542238,23.6006388275175,27.8368200529749));
#37403=CARTESIAN_POINT('Ctrl Pts',(19.6881825115154,23.7543320991532,27.6617032035706));
#37404=CARTESIAN_POINT('',(19.9952892223024,23.7543320991532,27.8173935619593));
#37405=CARTESIAN_POINT('Ctrl Pts',(19.9952892223024,23.7543320991532,27.8173935619593));
#37406=CARTESIAN_POINT('Ctrl Pts',(19.8484014534417,23.6006388275175,27.9132101820909));
#37407=CARTESIAN_POINT('Ctrl Pts',(19.70690406142,23.4543320991532,28.0055105959791));
#37408=CARTESIAN_POINT('',(20.2769374019214,23.7543320991532,27.9749354849866));
#37409=CARTESIAN_POINT('Origin',(16.1460502915689,23.7543320991532,35.0294657090004));
#37410=CARTESIAN_POINT('',(20.2675731631797,23.4543320991532,28.3191248667786));
#37411=CARTESIAN_POINT('Ctrl Pts',(20.2675731631797,23.4543320991532,28.3191248667786));
#37412=CARTESIAN_POINT('Ctrl Pts',(20.2721677663006,23.6006388275175,28.1502468990769));
#37413=CARTESIAN_POINT('Ctrl Pts',(20.2769374019214,23.7543320991532,27.9749354849866));
#37414=CARTESIAN_POINT('',(20.5703320308953,23.7543320991532,28.15513984452));
#37415=CARTESIAN_POINT('Ctrl Pts',(20.5703320308953,23.7543320991532,28.15513984452));
#37416=CARTESIAN_POINT('Ctrl Pts',(20.4161230749093,23.6006388275175,28.2386649259508));
#37417=CARTESIAN_POINT('Ctrl Pts',(20.2675731631797,23.4543320991532,28.3191248667786));
#37418=CARTESIAN_POINT('',(20.8382019201564,23.7543320991532,28.3351145011278));
#37419=CARTESIAN_POINT('Origin',(16.1460502915689,23.7543320991532,35.0294657090004));
#37420=CARTESIAN_POINT('',(20.8008142102322,23.4543320991532,28.6773953487548));
#37421=CARTESIAN_POINT('Ctrl Pts',(20.8008142102322,23.4543320991532,28.6773953487548));
#37422=CARTESIAN_POINT('Ctrl Pts',(20.8191586473445,23.6006388275175,28.5094538113677));
#37423=CARTESIAN_POINT('Ctrl Pts',(20.8382019201564,23.7543320991532,28.3351145011278));
#37424=CARTESIAN_POINT('',(21.1159319744681,23.7543320991532,28.538633631525));
#37425=CARTESIAN_POINT('Ctrl Pts',(21.1159319744681,23.7543320991532,28.538633631525));
#37426=CARTESIAN_POINT('Ctrl Pts',(20.9554280665162,23.6006388275175,28.6093113286187));
#37427=CARTESIAN_POINT('Ctrl Pts',(20.8008142102322,23.4543320991532,28.6773953487548));
#37428=CARTESIAN_POINT('',(21.3682409434536,23.7543320991532,28.7398433200673));
#37429=CARTESIAN_POINT('Origin',(16.1460502915689,23.7543320991532,35.0294657090004));
#37430=CARTESIAN_POINT('',(21.303078571388,23.4543320991532,29.0779378109605));
#37431=CARTESIAN_POINT('Ctrl Pts',(21.303078571388,23.4543320991532,29.0779378109605));
#37432=CARTESIAN_POINT('Ctrl Pts',(21.3350507632894,23.6006388275175,28.912050327111));
#37433=CARTESIAN_POINT('Ctrl Pts',(21.3682409434536,23.7543320991532,28.7398433200673));
#37434=CARTESIAN_POINT('',(21.6284581754139,23.7543320991532,28.9653228350936));
#37435=CARTESIAN_POINT('Ctrl Pts',(21.6284581754139,23.7543320991532,28.9653228350936));
#37436=CARTESIAN_POINT('Ctrl Pts',(21.4627274425222,23.6006388275175,29.022682799437));
#37437=CARTESIAN_POINT('Ctrl Pts',(21.303078571388,23.4543320991532,29.0779378109605));
#37438=CARTESIAN_POINT('',(21.8635271495634,23.7543320991532,29.1864285382904));
#37439=CARTESIAN_POINT('Origin',(16.1460502915689,23.7543320991532,35.0294657090004));
#37440=CARTESIAN_POINT('',(21.7710237601914,23.4543320991532,29.5180867093948));
#37441=CARTESIAN_POINT('Ctrl Pts',(21.7710237601914,23.4543320991532,29.5180867093948));
#37442=CARTESIAN_POINT('Ctrl Pts',(21.8164109372197,23.6006388275175,29.3553572329183));
#37443=CARTESIAN_POINT('Ctrl Pts',(21.8635271495634,23.7543320991532,29.1864285382904));
#37444=CARTESIAN_POINT('',(22.1044998564264,23.7543320991532,29.4323679089749));
#37445=CARTESIAN_POINT('Ctrl Pts',(22.1044998564264,23.7543320991532,29.4323679089749));
#37446=CARTESIAN_POINT('Ctrl Pts',(21.9346452092787,23.6006388275175,29.4760284194692));
#37447=CARTESIAN_POINT('Ctrl Pts',(21.7710237601914,23.4543320991532,29.5180867093948));
#37448=CARTESIAN_POINT('',(22.3207644905005,23.7543320991532,29.6718982048514));
#37449=CARTESIAN_POINT('Origin',(16.1460502915689,23.7543320991532,35.0294657090004));
#37450=CARTESIAN_POINT('',(22.2015356786164,23.4543320991532,29.9949129257578));
#37451=CARTESIAN_POINT('Ctrl Pts',(22.2015356786164,23.4543320991532,29.9949129257578));
#37452=CARTESIAN_POINT('Ctrl Pts',(22.2600357965969,23.6006388275175,29.836424394472));
#37453=CARTESIAN_POINT('Ctrl Pts',(22.3207644905005,23.7543320991532,29.6718982048514));
#37454=CARTESIAN_POINT('',(22.5408890386598,23.7543320991532,29.9366607452593));
#37455=CARTESIAN_POINT('Ctrl Pts',(22.5408890386598,23.7543320991532,29.9366607452593));
#37456=CARTESIAN_POINT('Ctrl Pts',(22.3680408319087,23.6006388275175,29.9663312484104));
#37457=CARTESIAN_POINT('Ctrl Pts',(22.2015356786164,23.4543320991532,29.9949129257578));
#37458=CARTESIAN_POINT('',(22.7369101271998,23.7543320991532,30.193021599216));
#37459=CARTESIAN_POINT('Origin',(16.1460502915689,23.7543320991532,35.0294657090004));
#37460=CARTESIAN_POINT('',(22.5917493408753,23.4543320991532,30.5052432602507));
#37461=CARTESIAN_POINT('Ctrl Pts',(22.5917493408753,23.4543320991532,30.5052432602507));
#37462=CARTESIAN_POINT('Ctrl Pts',(22.6629730911747,23.6006388275175,30.3520503891823));
#37463=CARTESIAN_POINT('Ctrl Pts',(22.7369101271998,23.7543320991532,30.193021599216));
#37464=CARTESIAN_POINT('',(22.9347216241054,23.7543320991532,30.4748453583237));
#37465=CARTESIAN_POINT('Ctrl Pts',(22.9347216241053,23.7543320991532,30.4748453583237));
#37466=CARTESIAN_POINT('Ctrl Pts',(22.7600301340489,23.6006388275175,30.4903284018285));
#37467=CARTESIAN_POINT('Ctrl Pts',(22.5917493408753,23.4543320991532,30.5052432602507));
#37468=CARTESIAN_POINT('',(23.1091946791084,23.7543320991532,30.7463307311742));
#37469=CARTESIAN_POINT('Origin',(16.1460502915689,23.7543320991532,35.0294657090004));
#37470=CARTESIAN_POINT('',(22.9390679394266,23.4543320991532,31.0456815486958));
#37471=CARTESIAN_POINT('Ctrl Pts',(22.9390679394266,23.4543320991532,31.0456815486957));
#37472=CARTESIAN_POINT('Ctrl Pts',(23.0225413397378,23.6006388275175,30.8988038111267));
#37473=CARTESIAN_POINT('Ctrl Pts',(23.1091946791084,23.7543320991532,30.7463307311742));
#37474=CARTESIAN_POINT('',(23.2833767218848,23.7543320991532,31.0433402183623));
#37475=CARTESIAN_POINT('Ctrl Pts',(23.2833767218848,23.7543320991532,31.0433402183623));
#37476=CARTESIAN_POINT('Ctrl Pts',(23.1080044915673,23.6006388275175,31.0445327651209));
#37477=CARTESIAN_POINT('Ctrl Pts',(22.9390679394266,23.4543320991532,31.0456815486958));
#37478=CARTESIAN_POINT('',(23.4351406539558,23.7543320991532,31.3281434197422));
#37479=CARTESIAN_POINT('Origin',(16.1460502915689,23.7543320991532,35.0294657090004));
#37480=CARTESIAN_POINT('',(23.2411801263005,23.4543320991532,31.6126312634495));
#37481=CARTESIAN_POINT('Ctrl Pts',(23.2411801263005,23.4543320991532,31.6126312634495));
#37482=CARTESIAN_POINT('Ctrl Pts',(23.3363476749164,23.6006388275175,31.4730461064903));
#37483=CARTESIAN_POINT('Ctrl Pts',(23.4351406539558,23.7543320991532,31.3281434197422));
#37484=CARTESIAN_POINT('',(23.5845340898465,23.7543320991532,31.6383620858768));
#37485=CARTESIAN_POINT('Ctrl Pts',(23.5845340898465,23.7543320991532,31.6383620858768));
#37486=CARTESIAN_POINT('Ctrl Pts',(23.4096481925263,23.6006388275175,31.6252561996872));
#37487=CARTESIAN_POINT('Ctrl Pts',(23.2411801263005,23.4543320991532,31.6126312634495));
#37488=CARTESIAN_POINT('',(23.7125789350568,23.7543320991532,31.9345877974701));
#37489=CARTESIAN_POINT('Origin',(16.1460502915689,23.7543320991532,35.0294657090004));
#37490=CARTESIAN_POINT('',(23.4960753947382,23.4543320991532,32.2023194477005));
#37491=CARTESIAN_POINT('Ctrl Pts',(23.4960753947382,23.4543320991532,32.2023194477005));
#37492=CARTESIAN_POINT('Ctrl Pts',(23.6023037673244,23.6006388275175,32.0709557875407));
#37493=CARTESIAN_POINT('Ctrl Pts',(23.7125789350568,23.7543320991532,31.9345877974701));
#37494=CARTESIAN_POINT('',(23.8361895753941,23.7543320991532,32.2559511885104));
#37495=CARTESIAN_POINT('Ctrl Pts',(23.8361895753941,23.7543320991532,32.2559511885104));
#37496=CARTESIAN_POINT('Ctrl Pts',(23.6629538478638,23.6006388275175,32.2286340868829));
#37497=CARTESIAN_POINT('Ctrl Pts',(23.4960753947382,23.4543320991532,32.2023194477005));
#37498=CARTESIAN_POINT('',(23.9396632164247,23.7543320991532,32.5616280770803));
#37499=CARTESIAN_POINT('Origin',(16.1460502915689,23.7543320991532,35.0294657090004));
#37500=CARTESIAN_POINT('',(23.7020574587831,23.4543320991532,32.8108218238741));
#37501=CARTESIAN_POINT('Ctrl Pts',(23.7020574587831,23.4543320991532,32.8108218238741));
#37502=CARTESIAN_POINT('Ctrl Pts',(23.8186397230465,23.6006388275175,32.6885538639986));
#37503=CARTESIAN_POINT('Ctrl Pts',(23.9396632164247,23.7543320991532,32.5616280770803));
#37504=CARTESIAN_POINT('',(24.0366684527916,23.7543320991532,32.8919975726802));
#37505=CARTESIAN_POINT('Ctrl Pts',(24.0366684527916,23.7543320991532,32.8919975726803));
#37506=CARTESIAN_POINT('Ctrl Pts',(23.8662357502358,23.6006388275175,32.8506510464192));
#37507=CARTESIAN_POINT('Ctrl Pts',(23.7020574587831,23.4543320991532,32.8108218238741));
#37508=CARTESIAN_POINT('',(24.1148822896334,23.7543320991532,33.2050914089663));
#37509=CARTESIAN_POINT('Origin',(16.1460502915689,23.7543320991532,35.0294657090004));
#37510=CARTESIAN_POINT('',(23.8577555417836,23.4543320991532,33.4340889090527));
#37511=CARTESIAN_POINT('Ctrl Pts',(23.8577555417836,23.4543320991532,33.4340889090527));
#37512=CARTESIAN_POINT('Ctrl Pts',(23.9839158619903,23.6006388275175,33.3217303225617));
#37513=CARTESIAN_POINT('Ctrl Pts',(24.1148822896334,23.7543320991532,33.2050914089663));
#37514=CARTESIAN_POINT('',(24.1846365681864,23.7543320991532,33.5422684546398));
#37515=CARTESIAN_POINT('Ctrl Pts',(24.1846365681864,23.7543320991532,33.5422684546398));
#37516=CARTESIAN_POINT('Ctrl Pts',(24.0181410921214,23.6006388275175,33.4871676580557));
#37517=CARTESIAN_POINT('Ctrl Pts',(23.8577555417836,23.4543320991532,33.4340889090527));
#37518=CARTESIAN_POINT('',(24.2370701006596,23.7543320991532,33.8606956508185));
#37519=CARTESIAN_POINT('Origin',(16.1460502915689,23.7543320991532,35.0294657090004));
#37520=CARTESIAN_POINT('',(23.9621334986858,23.4543320991532,34.0679729636163));
#37521=CARTESIAN_POINT('Ctrl Pts',(23.9621334986858,23.4543320991532,34.0679729636163));
#37522=CARTESIAN_POINT('Ctrl Pts',(24.0970322987197,23.6006388275175,33.9662714783651));
#37523=CARTESIAN_POINT('Ctrl Pts',(24.2370701006596,23.7543320991532,33.8606956508185));
#37524=CARTESIAN_POINT('',(24.2791092181837,23.7543320991532,34.2024363889569));
#37525=CARTESIAN_POINT('Ctrl Pts',(24.2791092181837,23.7543320991532,34.2024363889569));
#37526=CARTESIAN_POINT('Ctrl Pts',(24.1176589685329,23.6006388275175,34.1339480087601));
#37527=CARTESIAN_POINT('Ctrl Pts',(23.9621334986858,23.4543320991532,34.0679729636163));
#37528=CARTESIAN_POINT('',(24.3054135097807,23.7543320991532,34.5240778645745));
#37529=CARTESIAN_POINT('Origin',(16.1460502915689,23.7543320991532,35.0294657090004));
#37530=CARTESIAN_POINT('',(24.0144967114075,23.4543320991532,34.7082555937653));
#37531=CARTESIAN_POINT('Ctrl Pts',(24.0144967114075,23.4543320991532,34.7082555937653));
#37532=CARTESIAN_POINT('Ctrl Pts',(24.1572362620112,23.6006388275175,34.6178880163586));
#37533=CARTESIAN_POINT('Ctrl Pts',(24.3054135097807,23.7543320991532,34.5240778645745));
#37534=CARTESIAN_POINT('',(24.3194577028847,23.7543320991532,34.8681080669487));
#37535=CARTESIAN_POINT('Ctrl Pts',(24.3194577028847,23.7543320991532,34.8681080669487));
#37536=CARTESIAN_POINT('Ctrl Pts',(24.164127104422,23.6006388275175,34.7866878820095));
#37537=CARTESIAN_POINT('Ctrl Pts',(24.0144967114075,23.4543320991532,34.7082555937653));
#37538=CARTESIAN_POINT('',(24.3194577028847,23.7543320991532,35.1908233510519));
#37539=CARTESIAN_POINT('Origin',(16.1460502915689,23.7543320991532,35.0294657090004));
#37540=CARTESIAN_POINT('',(24.0144967114075,23.4543320991532,35.3506758242353));
#37541=CARTESIAN_POINT('Ctrl Pts',(24.0144967114075,23.4543320991532,35.3506758242353));
#37542=CARTESIAN_POINT('Ctrl Pts',(24.164127104422,23.6006388275175,35.2722435359911));
#37543=CARTESIAN_POINT('Ctrl Pts',(24.3194577028847,23.7543320991532,35.1908233510519));
#37544=CARTESIAN_POINT('',(24.3054135097807,23.7543320991532,35.5348535534261));
#37545=CARTESIAN_POINT('Ctrl Pts',(24.3054135097807,23.7543320991532,35.5348535534261));
#37546=CARTESIAN_POINT('Ctrl Pts',(24.1572362620112,23.6006388275175,35.441043401642));
#37547=CARTESIAN_POINT('Ctrl Pts',(24.0144967114075,23.4543320991532,35.3506758242353));
#37548=CARTESIAN_POINT('',(24.2791092181837,23.7543320991532,35.8564950290437));
#37549=CARTESIAN_POINT('Origin',(16.1460502915689,23.7543320991532,35.0294657090004));
#37550=CARTESIAN_POINT('',(23.9621334986858,23.4543320991532,35.9909584543843));
#37551=CARTESIAN_POINT('Ctrl Pts',(23.9621334986858,23.4543320991532,35.9909584543843));
#37552=CARTESIAN_POINT('Ctrl Pts',(24.1176589685329,23.6006388275175,35.9249834092406));
#37553=CARTESIAN_POINT('Ctrl Pts',(24.2791092181837,23.7543320991532,35.8564950290437));
#37554=CARTESIAN_POINT('',(24.2370701006596,23.7543320991532,36.1982357671821));
#37555=CARTESIAN_POINT('Ctrl Pts',(24.2370701006596,23.7543320991532,36.1982357671821));
#37556=CARTESIAN_POINT('Ctrl Pts',(24.0970322987197,23.6006388275175,36.0926599396356));
#37557=CARTESIAN_POINT('Ctrl Pts',(23.9621334986858,23.4543320991532,35.9909584543843));
#37558=CARTESIAN_POINT('',(24.1846365681864,23.7543320991532,36.5166629633608));
#37559=CARTESIAN_POINT('Origin',(16.1460502915689,23.7543320991532,35.0294657090004));
#37560=CARTESIAN_POINT('',(23.8577555417836,23.4543320991532,36.6248425089479));
#37561=CARTESIAN_POINT('Ctrl Pts',(23.8577555417836,23.4543320991532,36.6248425089479));
#37562=CARTESIAN_POINT('Ctrl Pts',(24.0181410921214,23.6006388275175,36.5717637599449));
#37563=CARTESIAN_POINT('Ctrl Pts',(24.1846365681864,23.7543320991532,36.5166629633608));
#37564=CARTESIAN_POINT('',(24.1148822896334,23.7543320991532,36.8538400090343));
#37565=CARTESIAN_POINT('Ctrl Pts',(24.1148822896334,23.7543320991532,36.8538400090343));
#37566=CARTESIAN_POINT('Ctrl Pts',(23.9839158619903,23.6006388275175,36.7372010954389));
#37567=CARTESIAN_POINT('Ctrl Pts',(23.8577555417836,23.4543320991532,36.624842508948));
#37568=CARTESIAN_POINT('',(24.0366684527916,23.7543320991532,37.1669338453204));
#37569=CARTESIAN_POINT('Origin',(16.1460502915689,23.7543320991532,35.0294657090004));
#37570=CARTESIAN_POINT('',(23.7020574587831,23.4543320991532,37.2481095941266));
#37571=CARTESIAN_POINT('Ctrl Pts',(23.7020574587831,23.4543320991532,37.2481095941266));
#37572=CARTESIAN_POINT('Ctrl Pts',(23.8662357502359,23.6006388275175,37.2082803715815));
#37573=CARTESIAN_POINT('Ctrl Pts',(24.0366684527916,23.7543320991532,37.1669338453204));
#37574=CARTESIAN_POINT('',(23.9396632164247,23.7543320991532,37.4973033409204));
#37575=CARTESIAN_POINT('Ctrl Pts',(23.9396632164247,23.7543320991532,37.4973033409204));
#37576=CARTESIAN_POINT('Ctrl Pts',(23.8186397230465,23.6006388275175,37.370377554002));
#37577=CARTESIAN_POINT('Ctrl Pts',(23.7020574587831,23.4543320991532,37.2481095941266));
#37578=CARTESIAN_POINT('',(23.8361895753942,23.7543320991532,37.8029802294902));
#37579=CARTESIAN_POINT('Origin',(16.1460502915689,23.7543320991532,35.0294657090004));
#37580=CARTESIAN_POINT('',(23.4960753947382,23.4543320991532,37.8566119703002));
#37581=CARTESIAN_POINT('Ctrl Pts',(23.4960753947382,23.4543320991532,37.8566119703002));
#37582=CARTESIAN_POINT('Ctrl Pts',(23.6629538478638,23.6006388275175,37.8302973311177));
#37583=CARTESIAN_POINT('Ctrl Pts',(23.8361895753942,23.7543320991532,37.8029802294902));
#37584=CARTESIAN_POINT('',(23.7125789350568,23.7543320991532,38.1243436205306));
#37585=CARTESIAN_POINT('Ctrl Pts',(23.7125789350568,23.7543320991532,38.1243436205306));
#37586=CARTESIAN_POINT('Ctrl Pts',(23.6023037673244,23.6006388275175,37.9879756304599));
#37587=CARTESIAN_POINT('Ctrl Pts',(23.4960753947382,23.4543320991532,37.8566119703002));
#37588=CARTESIAN_POINT('',(23.5845340898466,23.7543320991532,38.4205693321238));
#37589=CARTESIAN_POINT('Origin',(16.1460502915689,23.7543320991532,35.0294657090004));
#37590=CARTESIAN_POINT('',(23.2411801263005,23.4543320991532,38.4463001545511));
#37591=CARTESIAN_POINT('Ctrl Pts',(23.2411801263005,23.4543320991532,38.4463001545511));
#37592=CARTESIAN_POINT('Ctrl Pts',(23.4096481925264,23.6006388275175,38.4336752183134));
#37593=CARTESIAN_POINT('Ctrl Pts',(23.5845340898466,23.7543320991532,38.4205693321238));
#37594=CARTESIAN_POINT('',(23.4351406539558,23.7543320991532,38.7307879982584));
#37595=CARTESIAN_POINT('Ctrl Pts',(23.4351406539558,23.7543320991532,38.7307879982584));
#37596=CARTESIAN_POINT('Ctrl Pts',(23.3363476749164,23.6006388275175,38.5858853115103));
#37597=CARTESIAN_POINT('Ctrl Pts',(23.2411801263005,23.4543320991532,38.4463001545511));
#37598=CARTESIAN_POINT('',(23.2833767218849,23.7543320991532,39.0155911996383));
#37599=CARTESIAN_POINT('Origin',(16.1460502915689,23.7543320991532,35.0294657090004));
#37600=CARTESIAN_POINT('',(22.9390679394267,23.4543320991532,39.0132498693049));
#37601=CARTESIAN_POINT('Ctrl Pts',(22.9390679394267,23.4543320991532,39.0132498693049));
#37602=CARTESIAN_POINT('Ctrl Pts',(23.1080044915674,23.6006388275175,39.0143986528797));
#37603=CARTESIAN_POINT('Ctrl Pts',(23.2833767218849,23.7543320991532,39.0155911996383));
#37604=CARTESIAN_POINT('',(23.1091946791084,23.7543320991532,39.3126006868265));
#37605=CARTESIAN_POINT('Ctrl Pts',(23.1091946791084,23.7543320991532,39.3126006868265));
#37606=CARTESIAN_POINT('Ctrl Pts',(23.0225413397378,23.6006388275175,39.1601276068739));
#37607=CARTESIAN_POINT('Ctrl Pts',(22.9390679394267,23.4543320991532,39.0132498693049));
#37608=CARTESIAN_POINT('',(22.9347216241054,23.7543320991532,39.584086059677));
#37609=CARTESIAN_POINT('Origin',(16.1460502915689,23.7543320991532,35.0294657090004));
#37610=CARTESIAN_POINT('',(22.5917493408754,23.4543320991532,39.55368815775));
#37611=CARTESIAN_POINT('Ctrl Pts',(22.5917493408754,23.4543320991532,39.55368815775));
#37612=CARTESIAN_POINT('Ctrl Pts',(22.760030134049,23.6006388275175,39.5686030161721));
#37613=CARTESIAN_POINT('Ctrl Pts',(22.9347216241054,23.7543320991532,39.584086059677));
#37614=CARTESIAN_POINT('',(22.7369101271999,23.7543320991532,39.8659098187846));
#37615=CARTESIAN_POINT('Ctrl Pts',(22.7369101271999,23.7543320991532,39.8659098187846));
#37616=CARTESIAN_POINT('Ctrl Pts',(22.6629730911748,23.6006388275175,39.7068810288184));
#37617=CARTESIAN_POINT('Ctrl Pts',(22.5917493408754,23.4543320991532,39.55368815775));
#37618=CARTESIAN_POINT('',(22.5408890386598,23.7543320991532,40.1222706727414));
#37619=CARTESIAN_POINT('Origin',(16.1460502915689,23.7543320991532,35.0294657090004));
#37620=CARTESIAN_POINT('',(22.2015356786164,23.4543320991532,40.0640184922428));
#37621=CARTESIAN_POINT('Ctrl Pts',(22.2015356786164,23.4543320991532,40.0640184922428));
#37622=CARTESIAN_POINT('Ctrl Pts',(22.3680408319088,23.6006388275175,40.0926001695902));
#37623=CARTESIAN_POINT('Ctrl Pts',(22.5408890386598,23.7543320991532,40.1222706727414));
#37624=CARTESIAN_POINT('',(22.3207644905006,23.7543320991532,40.3870332131493));
#37625=CARTESIAN_POINT('Ctrl Pts',(22.3207644905006,23.7543320991532,40.3870332131493));
#37626=CARTESIAN_POINT('Ctrl Pts',(22.260035796597,23.6006388275175,40.2225070235287));
#37627=CARTESIAN_POINT('Ctrl Pts',(22.2015356786164,23.4543320991532,40.0640184922428));
#37628=CARTESIAN_POINT('',(22.1044998564265,23.7543320991532,40.6265635090257));
#37629=CARTESIAN_POINT('Origin',(16.1460502915689,23.7543320991532,35.0294657090004));
#37630=CARTESIAN_POINT('',(21.7710237601915,23.4543320991532,40.5408447086059));
#37631=CARTESIAN_POINT('Ctrl Pts',(21.7710237601915,23.4543320991532,40.5408447086059));
#37632=CARTESIAN_POINT('Ctrl Pts',(21.9346452092787,23.6006388275175,40.5829029985315));
#37633=CARTESIAN_POINT('Ctrl Pts',(22.1044998564265,23.7543320991532,40.6265635090257));
#37634=CARTESIAN_POINT('',(21.8635271495635,23.7543320991532,40.8725028797102));
#37635=CARTESIAN_POINT('Ctrl Pts',(21.8635271495635,23.7543320991532,40.8725028797102));
#37636=CARTESIAN_POINT('Ctrl Pts',(21.8164109372198,23.6006388275175,40.7035741850823));
#37637=CARTESIAN_POINT('Ctrl Pts',(21.7710237601915,23.4543320991532,40.5408447086059));
#37638=CARTESIAN_POINT('',(21.628458175414,23.7543320991532,41.0936085829071));
#37639=CARTESIAN_POINT('Origin',(16.1460502915689,23.7543320991532,35.0294657090004));
#37640=CARTESIAN_POINT('',(21.3030785713881,23.4543320991532,40.9809936070401));
#37641=CARTESIAN_POINT('Ctrl Pts',(21.3030785713881,23.4543320991532,40.9809936070401));
#37642=CARTESIAN_POINT('Ctrl Pts',(21.4627274425223,23.6006388275175,41.0362486185636));
#37643=CARTESIAN_POINT('Ctrl Pts',(21.628458175414,23.7543320991532,41.0936085829071));
#37644=CARTESIAN_POINT('',(21.3682409434537,23.7543320991532,41.3190880979334));
#37645=CARTESIAN_POINT('Ctrl Pts',(21.3682409434537,23.7543320991532,41.3190880979334));
#37646=CARTESIAN_POINT('Ctrl Pts',(21.3350507632894,23.6006388275175,41.1468810908896));
#37647=CARTESIAN_POINT('Ctrl Pts',(21.3030785713881,23.4543320991532,40.9809936070401));
#37648=CARTESIAN_POINT('',(21.1159319744682,23.7543320991532,41.5202977864757));
#37649=CARTESIAN_POINT('Origin',(16.1460502915689,23.7543320991532,35.0294657090004));
#37650=CARTESIAN_POINT('',(20.8008142102323,23.4543320991532,41.3815360692459));
#37651=CARTESIAN_POINT('Ctrl Pts',(20.8008142102323,23.4543320991532,41.3815360692459));
#37652=CARTESIAN_POINT('Ctrl Pts',(20.9554280665163,23.6006388275175,41.449620089382));
#37653=CARTESIAN_POINT('Ctrl Pts',(21.1159319744682,23.7543320991532,41.5202977864757));
#37654=CARTESIAN_POINT('',(20.8382019201565,23.7543320991532,41.7238169168728));
#37655=CARTESIAN_POINT('Ctrl Pts',(20.8382019201565,23.7543320991532,41.7238169168728));
#37656=CARTESIAN_POINT('Ctrl Pts',(20.8191586473446,23.6006388275175,41.5494776066329));
#37657=CARTESIAN_POINT('Ctrl Pts',(20.8008142102323,23.4543320991532,41.3815360692459));
#37658=CARTESIAN_POINT('',(20.5703320308954,23.7543320991532,41.9037915734806));
#37659=CARTESIAN_POINT('Origin',(16.1460502915689,23.7543320991532,35.0294657090004));
#37660=CARTESIAN_POINT('',(20.2675731631798,23.4543320991532,41.7398065512221));
#37661=CARTESIAN_POINT('Ctrl Pts',(20.2675731631798,23.4543320991532,41.7398065512221));
#37662=CARTESIAN_POINT('Ctrl Pts',(20.4161230749094,23.6006388275175,41.8202664920499));
#37663=CARTESIAN_POINT('Ctrl Pts',(20.5703320308954,23.7543320991532,41.9037915734806));
#37664=CARTESIAN_POINT('',(20.2769374019215,23.7543320991532,42.0839959330141));
#37665=CARTESIAN_POINT('Ctrl Pts',(20.2769374019215,23.7543320991532,42.0839959330141));
#37666=CARTESIAN_POINT('Ctrl Pts',(20.2721677663007,23.6006388275175,41.9086845189237));
#37667=CARTESIAN_POINT('Ctrl Pts',(20.2675731631798,23.4543320991532,41.7398065512221));
#37668=CARTESIAN_POINT('',(19.9952892223025,23.7543320991532,42.2415378560414));
#37669=CARTESIAN_POINT('Origin',(16.1460502915689,23.7543320991532,35.0294657090004));
#37670=CARTESIAN_POINT('',(19.7069040614201,23.4543320991532,42.0534208220216));
#37671=CARTESIAN_POINT('Ctrl Pts',(19.7069040614201,23.4543320991532,42.0534208220216));
#37672=CARTESIAN_POINT('Ctrl Pts',(19.8484014534418,23.6006388275175,42.1457212359098));
#37673=CARTESIAN_POINT('Ctrl Pts',(19.9952892223025,23.7543320991532,42.2415378560414));
#37674=CARTESIAN_POINT('',(19.6881825115155,23.7543320991532,42.3972282144301));
#37675=CARTESIAN_POINT('Ctrl Pts',(19.6881825115155,23.7543320991532,42.3972282144301));
#37676=CARTESIAN_POINT('Ctrl Pts',(19.6977182542239,23.6006388275175,42.2221113650258));
#37677=CARTESIAN_POINT('Ctrl Pts',(19.7069040614201,23.4543320991532,42.0534208220216));
#37678=CARTESIAN_POINT('',(19.3946303637053,23.7543320991532,42.5312889883718));
#37679=CARTESIAN_POINT('Origin',(16.1460502915689,23.7543320991532,35.0294657090004));
#37680=CARTESIAN_POINT('',(19.1225380653216,23.4543320991532,42.3202918304149));
#37681=CARTESIAN_POINT('Ctrl Pts',(19.1225380653216,23.4543320991532,42.3202918304149));
#37682=CARTESIAN_POINT('Ctrl Pts',(19.256041295837,23.6006388275175,42.4238184733377));
#37683=CARTESIAN_POINT('Ctrl Pts',(19.3946303637053,23.7543320991532,42.5312889883718));
#37684=CARTESIAN_POINT('',(19.0758553155965,23.7543320991532,42.6614292519677));
#37685=CARTESIAN_POINT('Ctrl Pts',(19.0758553155965,23.7543320991532,42.6614292519677));
#37686=CARTESIAN_POINT('Ctrl Pts',(19.0996329778397,23.6006388275175,42.4876723409899));
#37687=CARTESIAN_POINT('Ctrl Pts',(19.1225380653216,23.4543320991532,42.3202918304149));
#37688=CARTESIAN_POINT('',(18.772352740706,23.7543320991532,42.7711167244916));
#37689=CARTESIAN_POINT('Origin',(16.1460502915689,23.7543320991532,35.0294657090004));
#37690=CARTESIAN_POINT('',(18.5183640341747,23.4543320991532,42.5386435938719));
#37691=CARTESIAN_POINT('Ctrl Pts',(18.5183640341747,23.4543320991532,42.5386435938719));
#37692=CARTESIAN_POINT('Ctrl Pts',(18.6429846612111,23.6006388275175,42.6527075131012));
#37693=CARTESIAN_POINT('Ctrl Pts',(18.772352740706,23.7543320991532,42.7711167244916));
#37694=CARTESIAN_POINT('',(18.4440307506264,23.7543320991532,42.8748408313122));
#37695=CARTESIAN_POINT('Ctrl Pts',(18.4440307506264,23.7543320991532,42.8748408313122));
#37696=CARTESIAN_POINT('Ctrl Pts',(18.4818920959851,23.6006388275175,42.7036001823356));
#37697=CARTESIAN_POINT('Ctrl Pts',(18.5183640341747,23.4543320991532,42.5386435938719));
#37698=CARTESIAN_POINT('',(18.1325975082171,23.7543320991532,42.9594250503859));
#37699=CARTESIAN_POINT('Origin',(16.1460502915689,23.7543320991532,35.0294657090004));
#37700=CARTESIAN_POINT('',(17.8984026464749,23.4543320991532,42.7070230174322));
#37701=CARTESIAN_POINT('Ctrl Pts',(17.8984026464749,23.4543320991532,42.7070230174322));
#37702=CARTESIAN_POINT('Ctrl Pts',(18.0133113403204,23.6006388275175,42.8308651364048));
#37703=CARTESIAN_POINT('Ctrl Pts',(18.1325975082171,23.7543320991532,42.9594250503859));
#37704=CARTESIAN_POINT('',(17.7969135048413,23.7543320991532,43.0360427336136));
#37705=CARTESIAN_POINT('Ctrl Pts',(17.7969135048413,23.7543320991532,43.0360427336136));
#37706=CARTESIAN_POINT('Ctrl Pts',(17.8486065723089,23.6006388275175,42.8684579249044));
#37707=CARTESIAN_POINT('Ctrl Pts',(17.8984026464749,23.4543320991532,42.7070230174322));
#37708=CARTESIAN_POINT('',(17.4796221317587,23.7543320991532,43.0949608052144));
#37709=CARTESIAN_POINT('Origin',(16.1460502915689,23.7543320991532,35.0294657090004));
#37710=CARTESIAN_POINT('',(17.2667796429711,23.4543320991532,42.8243095638127));
#37711=CARTESIAN_POINT('Ctrl Pts',(17.2667796429711,23.4543320991532,42.8243095638127));
#37712=CARTESIAN_POINT('Ctrl Pts',(17.3712117052267,23.6006388275175,42.9571057336593));
#37713=CARTESIAN_POINT('Ctrl Pts',(17.4796221317587,23.7543320991532,43.0949608052144));
#37714=CARTESIAN_POINT('',(17.1388100367452,23.7543320991532,43.1439621868083));
#37715=CARTESIAN_POINT('Ctrl Pts',(17.1388100367452,23.7543320991532,43.1439621868083));
#37716=CARTESIAN_POINT('Ctrl Pts',(17.2039908174864,23.6006388275175,42.981148467619));
#37717=CARTESIAN_POINT('Ctrl Pts',(17.2667796429711,23.4543320991532,42.8243095638127));
#37718=CARTESIAN_POINT('',(16.8177720547276,23.7543320991532,43.1768220208907));
#37719=CARTESIAN_POINT('Origin',(16.1460502915689,23.7543320991532,35.0294657090004));
#37720=CARTESIAN_POINT('',(16.627698370541,23.4543320991532,42.8897227103981));
#37721=CARTESIAN_POINT('Ctrl Pts',(16.627698370541,23.4543320991532,42.8897227103981));
#37722=CARTESIAN_POINT('Ctrl Pts',(16.7209588230625,23.6006388275175,43.0305891945183));
#37723=CARTESIAN_POINT('Ctrl Pts',(16.8177720547276,23.7543320991532,43.1768220208907));
#37724=CARTESIAN_POINT('',(16.4740999163387,23.7543320991532,43.1978810047409));
#37725=CARTESIAN_POINT('Ctrl Pts',(16.4740999163387,23.7543320991532,43.1978810047409));
#37726=CARTESIAN_POINT('Ctrl Pts',(16.5523346430118,23.6006388275175,43.0409218735102));
#37727=CARTESIAN_POINT('Ctrl Pts',(16.627698370541,23.4543320991532,42.8897227103981));
#37728=CARTESIAN_POINT('',(16.151451780189,23.7543320991532,43.2044639245305));
#37729=CARTESIAN_POINT('Origin',(16.1460502915689,23.7543320991532,35.0294657090004));
#37730=CARTESIAN_POINT('',(16.1460502915689,23.7445176916473,43.1946513014945));
#37731=CARTESIAN_POINT('Ctrl Pts',(16.151451780189,23.7543320991532,43.2044639245305));
#37732=CARTESIAN_POINT('Ctrl Pts',(16.1487494137306,23.7494210562869,43.199554666134));
#37733=CARTESIAN_POINT('Ctrl Pts',(16.1460502915689,23.7445176916473,43.1946513014945));
#37734=CARTESIAN_POINT('',(16.1460502915689,23.3543320991532,42.8044657090004));
#37735=CARTESIAN_POINT('',(16.1460502915689,23.7543320991532,43.2044657090004));
#37736=CARTESIAN_POINT('Origin',(16.1460502915689,23.3543320991532,35.0294657090004));
#37737=CARTESIAN_POINT('',(15.9854118096116,23.4543320991532,42.9028271434904));
#37738=CARTESIAN_POINT('Ctrl Pts',(16.1460502915689,23.7445176916473,43.1946513014945));
#37739=CARTESIAN_POINT('Ctrl Pts',(16.0642779822079,23.5959658936188,43.0460995034659));
#37740=CARTESIAN_POINT('Ctrl Pts',(15.9854118096116,23.4543320991532,42.9028271434904));
#37741=CARTESIAN_POINT('',(15.8072066798038,23.7543320991532,43.197440366574));
#37742=CARTESIAN_POINT('Ctrl Pts',(15.8072066798038,23.7543320991532,43.1974403665741));
#37743=CARTESIAN_POINT('Ctrl Pts',(15.8979747132106,23.6006388275175,43.047380360424));
#37744=CARTESIAN_POINT('Ctrl Pts',(15.9854118096116,23.4543320991532,42.9028271434904));
#37745=CARTESIAN_POINT('',(15.4850955596348,23.7543320991532,43.1777025638257));
#37746=CARTESIAN_POINT('Origin',(16.1460502915689,23.7543320991532,35.0294657090004));
#37747=CARTESIAN_POINT('',(15.3441942712763,23.4543320991532,42.8635356552493));
#37748=CARTESIAN_POINT('Ctrl Pts',(15.3441942712763,23.4543320991532,42.8635356552493));
#37749=CARTESIAN_POINT('Ctrl Pts',(15.4133280809849,23.6006388275175,43.017682970205));
#37750=CARTESIAN_POINT('Ctrl Pts',(15.4850955596348,23.7543320991532,43.1777025638257));
#37751=CARTESIAN_POINT('',(15.1425683915999,23.7543320991532,43.142643204682));
#37752=CARTESIAN_POINT('Ctrl Pts',(15.1425683915999,23.7543320991532,43.142643204682));
#37753=CARTESIAN_POINT('Ctrl Pts',(15.2452656854538,23.6006388275175,43.0004809481952));
#37754=CARTESIAN_POINT('Ctrl Pts',(15.3441942712763,23.4543320991532,42.8635356552493));
#37755=CARTESIAN_POINT('',(14.8231378837718,23.7543320991532,43.0967160312165));
#37756=CARTESIAN_POINT('Origin',(16.1460502915689,23.7543320991532,35.0294657090004));
#37757=CARTESIAN_POINT('',(14.708312952459,23.4543320991532,42.7721097240465));
#37758=CARTESIAN_POINT('Ctrl Pts',(14.708312952459,23.4543320991532,42.7721097240465));
#37759=CARTESIAN_POINT('Ctrl Pts',(14.7646522879162,23.6006388275175,42.9313791738262));
#37760=CARTESIAN_POINT('Ctrl Pts',(14.8231378837718,23.7543320991532,43.0967160312165));
#37761=CARTESIAN_POINT('',(14.4846081098775,23.7543320991532,43.0338541851362));
#37762=CARTESIAN_POINT('Ctrl Pts',(14.4846081098775,23.7543320991532,43.0338541851362));
#37763=CARTESIAN_POINT('Ctrl Pts',(14.5985512306316,23.6006388275175,42.9005357446746));
#37764=CARTESIAN_POINT('Ctrl Pts',(14.708312952459,23.4543320991532,42.7721097240465));
#37765=CARTESIAN_POINT('',(14.1699839717175,23.7543320991532,42.9620432787156));
#37766=CARTESIAN_POINT('Origin',(16.1460502915689,23.7543320991532,35.0294657090004));
#37767=CARTESIAN_POINT('',(14.0819995384235,23.4543320991532,42.6291577743698));
#37768=CARTESIAN_POINT('Ctrl Pts',(14.0819995384235,23.4543320991532,42.6291577743698));
#37769=CARTESIAN_POINT('Ctrl Pts',(14.1251694706472,23.6006388275175,42.7924894470628));
#37770=CARTESIAN_POINT('Ctrl Pts',(14.1699839717175,23.7543320991532,42.9620432787156));
#37771=CARTESIAN_POINT('',(13.8377044517555,23.7543320991532,42.8717972809129));
#37772=CARTESIAN_POINT('Ctrl Pts',(13.8377044517555,23.7543320991532,42.8717972809129));
#37773=CARTESIAN_POINT('Ctrl Pts',(13.9621351267406,23.6006388275175,42.7482098687017));
#37774=CARTESIAN_POINT('Ctrl Pts',(14.0819995384235,23.4543320991532,42.6291577743699));
#37775=CARTESIAN_POINT('',(13.5299804549939,23.7543320991532,42.7745805312714));
#37776=CARTESIAN_POINT('Origin',(16.1460502915689,23.7543320991532,35.0294657090004));
#37777=CARTESIAN_POINT('',(13.4694220416058,23.4543320991532,42.4356311278591));
#37778=CARTESIAN_POINT('Ctrl Pts',(13.4694220416058,23.4543320991532,42.4356311278591));
#37779=CARTESIAN_POINT('Ctrl Pts',(13.4991352818196,23.6006388275175,42.6019380781315));
#37780=CARTESIAN_POINT('Ctrl Pts',(13.5299804549938,23.7543320991532,42.7745805312714));
#37781=CARTESIAN_POINT('',(13.2061624543473,23.7543320991532,42.6575509539721));
#37782=CARTESIAN_POINT('Ctrl Pts',(13.2061624543473,23.7543320991532,42.6575509539721));
#37783=CARTESIAN_POINT('Ctrl Pts',(13.3402526179509,23.6006388275175,42.5445170238492));
#37784=CARTESIAN_POINT('Ctrl Pts',(13.4694220416058,23.4543320991532,42.4356311278591));
#37785=CARTESIAN_POINT('',(12.9073864514114,23.7543320991532,42.5355753225389));
#37786=CARTESIAN_POINT('Origin',(16.1460502915689,23.7543320991532,35.0294657090004));
#37787=CARTESIAN_POINT('',(12.8746570641791,23.4543320991532,42.1928176724172));
#37788=CARTESIAN_POINT('Ctrl Pts',(12.8746570641791,23.4543320991532,42.1928176724172));
#37789=CARTESIAN_POINT('Ctrl Pts',(12.8907158756716,23.6006388275175,42.3609931549536));
#37790=CARTESIAN_POINT('Ctrl Pts',(12.9073864514114,23.7543320991532,42.5355753225389));
#37791=CARTESIAN_POINT('',(12.5941849254484,23.7543320991532,42.3925409782716));
#37792=CARTESIAN_POINT('Ctrl Pts',(12.5941849254484,23.7543320991532,42.3925409782716));
#37793=CARTESIAN_POINT('Ctrl Pts',(12.7370422297551,23.6006388275175,42.2908127523925));
#37794=CARTESIAN_POINT('Ctrl Pts',(12.8746570641791,23.4543320991532,42.1928176724172));
#37795=CARTESIAN_POINT('',(12.3063452213433,23.7543320991532,42.2466181927493));
#37796=CARTESIAN_POINT('Origin',(16.1460502915689,23.7543320991532,35.0294657090004));
#37797=CARTESIAN_POINT('',(12.3016626689387,23.4543320991532,41.9023332915286));
#37798=CARTESIAN_POINT('Ctrl Pts',(12.3016626689387,23.4543320991532,41.9023332915286));
#37799=CARTESIAN_POINT('Ctrl Pts',(12.303960182969,23.6006388275175,42.0712581262397));
#37800=CARTESIAN_POINT('Ctrl Pts',(12.3063452213433,23.7543320991532,42.2466181927493));
#37801=CARTESIAN_POINT('',(12.0058444745445,23.7543320991532,42.0785309514759));
#37802=CARTESIAN_POINT('Ctrl Pts',(12.0058444745445,23.7543320991532,42.0785309514759));
#37803=CARTESIAN_POINT('Ctrl Pts',(12.156518227764,23.6006388275175,41.9887854144));
#37804=CARTESIAN_POINT('Ctrl Pts',(12.3016626689387,23.4543320991532,41.9023332915286));
#37805=CARTESIAN_POINT('',(11.7308565950109,23.7543320991532,41.9096321039267));
#37806=CARTESIAN_POINT('Origin',(16.1460502915689,23.7543320991532,35.0294657090004));
#37807=CARTESIAN_POINT('',(11.7542520390477,23.4543320991532,41.5661111108216));
#37808=CARTESIAN_POINT('Ctrl Pts',(11.7542520390477,23.4543320991532,41.5661111108216));
#37809=CARTESIAN_POINT('Ctrl Pts',(11.7427729660389,23.6006388275175,41.7346611308031));
#37810=CARTESIAN_POINT('Ctrl Pts',(11.7308565950109,23.7543320991532,41.9096321039267));
#37811=CARTESIAN_POINT('',(11.445056410267,23.7543320991532,41.7176105585055));
#37812=CARTESIAN_POINT('Ctrl Pts',(11.445056410267,23.7543320991532,41.7176105585055));
#37813=CARTESIAN_POINT('Ctrl Pts',(11.602543903431,23.6006388275175,41.6404449519749));
#37814=CARTESIAN_POINT('Ctrl Pts',(11.7542520390477,23.4543320991532,41.5661111108216));
#37815=CARTESIAN_POINT('',(11.1847503542733,23.7543320991532,41.5268596428934));
#37816=CARTESIAN_POINT('Origin',(16.1460502915689,23.7543320991532,35.0294657090004));
#37817=CARTESIAN_POINT('',(11.2360681019314,23.4543320991532,41.1863886334361));
#37818=CARTESIAN_POINT('Ctrl Pts',(11.2360681019314,23.4543320991532,41.1863886334361));
#37819=CARTESIAN_POINT('Ctrl Pts',(11.2108888332207,23.6006388275175,41.3534421661138));
#37820=CARTESIAN_POINT('Ctrl Pts',(11.1847503542733,23.7543320991532,41.5268596428934));
#37821=CARTESIAN_POINT('',(10.9155526846602,23.7543320991532,41.3121816650278));
#37822=CARTESIAN_POINT('Ctrl Pts',(10.9155526846602,23.7543320991532,41.3121816650278));
#37823=CARTESIAN_POINT('Ctrl Pts',(11.0788058644853,23.6006388275175,41.2481095134227));
#37824=CARTESIAN_POINT('Ctrl Pts',(11.2360681019314,23.4543320991532,41.1863886334361));
#37825=CARTESIAN_POINT('',(10.6716607460615,23.7543320991532,41.1008480972246));
#37826=CARTESIAN_POINT('Origin',(16.1460502915689,23.7543320991532,35.0294657090004));
#37827=CARTESIAN_POINT('',(10.7505592861972,23.4543320991532,40.7656928498092));
#37828=CARTESIAN_POINT('Ctrl Pts',(10.7505592861972,23.4543320991532,40.7656928498092));
#37829=CARTESIAN_POINT('Ctrl Pts',(10.7118473856633,23.6006388275175,40.930138181485));
#37830=CARTESIAN_POINT('Ctrl Pts',(10.6716607460615,23.7543320991532,41.1008480972246));
#37831=CARTESIAN_POINT('',(10.420857057656,23.7543320991532,40.864942333438));
#37832=CARTESIAN_POINT('Ctrl Pts',(10.420857057656,23.7543320991532,40.864942333438));
#37833=CARTESIAN_POINT('Ctrl Pts',(10.5887895011653,23.6006388275175,40.8143900263561));
#37834=CARTESIAN_POINT('Ctrl Pts',(10.7505592861972,23.4543320991532,40.7656928498093));
#37835=CARTESIAN_POINT('',(10.1950022970645,23.7543320991532,40.6344325034697));
#37836=CARTESIAN_POINT('Origin',(16.1460502915689,23.7543320991532,35.0294657090004));
#37837=CARTESIAN_POINT('',(10.3009565729103,23.4543320991532,40.3068234209711));
#37838=CARTESIAN_POINT('Ctrl Pts',(10.3009565729103,23.4543320991532,40.3068234209712));
#37839=CARTESIAN_POINT('Ctrl Pts',(10.2489696618645,23.6006388275175,40.4675661950943));
#37840=CARTESIAN_POINT('Ctrl Pts',(10.1950022970645,23.7543320991532,40.6344325034697));
#37841=CARTESIAN_POINT('',(9.96426164703311,23.7543320991532,40.3788688676983));
#37842=CARTESIAN_POINT('Ctrl Pts',(9.9642616470331,23.7543320991532,40.3788688676983));
#37843=CARTESIAN_POINT('Ctrl Pts',(10.135755791522,23.6006388275175,40.3421728224027));
#37844=CARTESIAN_POINT('Ctrl Pts',(10.3009565729103,23.4543320991532,40.3068234209712));
#37845=CARTESIAN_POINT('',(9.75794709061699,23.7543320991532,40.1307167804521));
#37846=CARTESIAN_POINT('Origin',(16.1460502915689,23.7543320991532,35.0294657090004));
#37847=CARTESIAN_POINT('',(9.89025199394856,23.4543320991532,39.8128340472626));
#37848=CARTESIAN_POINT('Ctrl Pts',(9.89025199394855,23.4543320991532,39.8128340472626));
#37849=CARTESIAN_POINT('Ctrl Pts',(9.82533603670643,23.6006388275175,39.968804547192));
#37850=CARTESIAN_POINT('Ctrl Pts',(9.75794709061698,23.7543320991532,40.1307167804521));
#37851=CARTESIAN_POINT('',(9.54880501991626,23.7543320991532,39.857196006527));
#37852=CARTESIAN_POINT('Ctrl Pts',(9.54880501991626,23.7543320991532,39.857196006527));
#37853=CARTESIAN_POINT('Ctrl Pts',(9.72271960014766,23.6006388275175,39.8346004291447));
#37854=CARTESIAN_POINT('Ctrl Pts',(9.89025199394855,23.4543320991532,39.8128340472626));
#37855=CARTESIAN_POINT('',(9.36340365700901,23.7543320991532,39.5930530732011));
#37856=CARTESIAN_POINT('Origin',(16.1460502915689,23.7543320991532,35.0294657090004));
#37857=CARTESIAN_POINT('',(9.52117872052339,23.4543320991532,39.2870121464632));
#37858=CARTESIAN_POINT('Ctrl Pts',(9.52117872052339,23.4543320991532,39.2870121464632));
#37859=CARTESIAN_POINT('Ctrl Pts',(9.44376572207008,23.6006388275175,39.4371724142552));
#37860=CARTESIAN_POINT('Ctrl Pts',(9.36340365700902,23.7543320991532,39.5930530732011));
#37861=CARTESIAN_POINT('',(9.17725197161341,23.7543320991532,39.303395396745));
#37862=CARTESIAN_POINT('Ctrl Pts',(9.17725197161342,23.7543320991532,39.303395396745));
#37863=CARTESIAN_POINT('Ctrl Pts',(9.3524296147498,23.6006388275175,39.2950506571155));
#37864=CARTESIAN_POINT('Ctrl Pts',(9.52117872052339,23.4543320991532,39.2870121464632));
#37865=CARTESIAN_POINT('',(9.01399761769611,23.7543320991532,39.0250194449803));
#37866=CARTESIAN_POINT('Origin',(16.1460502915689,23.7543320991532,35.0294657090004));
#37867=CARTESIAN_POINT('',(9.19619287437666,23.4543320991532,38.7328569765682));
#37868=CARTESIAN_POINT('Ctrl Pts',(9.19619287437665,23.4543320991532,38.7328569765682));
#37869=CARTESIAN_POINT('Ctrl Pts',(9.10679800544461,23.6006388275175,38.8762077204153));
#37870=CARTESIAN_POINT('Ctrl Pts',(9.01399761769611,23.7543320991532,39.0250194449803));
#37871=CARTESIAN_POINT('',(8.85207512635908,23.7543320991532,38.7211524900399));
#37872=CARTESIAN_POINT('Ctrl Pts',(8.85207512635908,23.7543320991532,38.7211524900399));
#37873=CARTESIAN_POINT('Ctrl Pts',(9.02735005408766,23.6006388275175,38.7271141210286));
#37874=CARTESIAN_POINT('Ctrl Pts',(9.19619287437665,23.4543320991532,38.7328569765682));
#37875=CARTESIAN_POINT('',(8.71205421222197,23.7543320991532,38.4303960658666));
#37876=CARTESIAN_POINT('Origin',(16.1460502915689,23.7543320991532,35.0294657090004));
#37877=CARTESIAN_POINT('',(8.91745718269558,23.4543320991532,38.154056348804));
#37878=CARTESIAN_POINT('Ctrl Pts',(8.91745718269558,23.4543320991532,38.154056348804));
#37879=CARTESIAN_POINT('Ctrl Pts',(8.81667535138843,23.6006388275175,38.2896435931571));
#37880=CARTESIAN_POINT('Ctrl Pts',(8.71205421222197,23.7543320991532,38.4303960658666));
#37881=CARTESIAN_POINT('',(8.57543848240802,23.7543320991532,38.1143420168924));
#37882=CARTESIAN_POINT('Ctrl Pts',(8.57543848240802,23.7543320991532,38.1143420168924));
#37883=CARTESIAN_POINT('Ctrl Pts',(8.74964426900309,23.6006388275175,38.1345703448287));
#37884=CARTESIAN_POINT('Ctrl Pts',(8.91745718269558,23.4543320991532,38.154056348804));
#37885=CARTESIAN_POINT('',(8.45958282413287,23.7543320991532,37.8131400563419));
#37886=CARTESIAN_POINT('Origin',(16.1460502915689,23.7543320991532,35.0294657090004));
#37887=CARTESIAN_POINT('',(8.68682658552014,23.4543320991532,37.5544620858532));
#37888=CARTESIAN_POINT('Ctrl Pts',(8.68682658552015,23.4543320991532,37.5544620858532));
#37889=CARTESIAN_POINT('Ctrl Pts',(8.57532847829742,23.6006388275175,37.6813835199714));
#37890=CARTESIAN_POINT('Ctrl Pts',(8.45958282413287,23.7543320991532,37.8131400563418));
#37891=CARTESIAN_POINT('',(8.3491830109839,23.7543320991532,37.4870022008846));
#37892=CARTESIAN_POINT('Ctrl Pts',(8.3491830109839,23.7543320991532,37.4870022008846));
#37893=CARTESIAN_POINT('Ctrl Pts',(8.5211603456776,23.6006388275175,37.5213626095835));
#37894=CARTESIAN_POINT('Ctrl Pts',(8.68682658552015,23.4543320991532,37.5544620858532));
#37895=CARTESIAN_POINT('',(8.25826360886169,23.7543320991532,37.1773591533095));
#37896=CARTESIAN_POINT('Origin',(16.1460502915689,23.7543320991532,35.0294657090004));
#37897=CARTESIAN_POINT('',(8.50583589142318,23.4543320991532,36.9380643886094));
#37898=CARTESIAN_POINT('Ctrl Pts',(8.50583589142318,23.4543320991532,36.9380643886094));
#37899=CARTESIAN_POINT('Ctrl Pts',(8.38436350979254,23.6006388275175,37.0554753712894));
#37900=CARTESIAN_POINT('Ctrl Pts',(8.25826360886169,23.7543320991532,37.1773591533095));
#37901=CARTESIAN_POINT('',(8.17481440491953,23.7543320991532,36.8433078849883));
#37902=CARTESIAN_POINT('Ctrl Pts',(8.17481440491953,23.7543320991532,36.8433078849883));
#37903=CARTESIAN_POINT('Ctrl Pts',(8.34341880692372,23.6006388275175,36.8915717115991));
#37904=CARTESIAN_POINT('Ctrl Pts',(8.50583589142317,23.4543320991532,36.9380643886094));
#37905=CARTESIAN_POINT('',(8.10943631257072,23.7543320991532,36.5272843737828));
#37906=CARTESIAN_POINT('Origin',(16.1460502915689,23.7543320991532,35.0294657090004));
#37907=CARTESIAN_POINT('',(8.37568956361253,23.4543320991532,36.3089652820495));
#37908=CARTESIAN_POINT('Ctrl Pts',(8.37568956361253,23.4543320991532,36.3089652820495));
#37909=CARTESIAN_POINT('Ctrl Pts',(8.24505128623221,23.6006388275175,36.4160844625728));
#37910=CARTESIAN_POINT('Ctrl Pts',(8.10943631257073,23.7543320991532,36.5272843737828));
#37911=CARTESIAN_POINT('',(8.05349305851946,23.7543320991532,36.1875427486737));
#37912=CARTESIAN_POINT('Ctrl Pts',(8.05349305851946,23.7543320991532,36.1875427486737));
#37913=CARTESIAN_POINT('Ctrl Pts',(8.21760249335658,23.6006388275175,36.2493888053932));
#37914=CARTESIAN_POINT('Ctrl Pts',(8.37568956361253,23.4543320991532,36.3089652820495));
#37915=CARTESIAN_POINT('',(8.01409135636202,23.7543320991532,35.8672418581646));
#37916=CARTESIAN_POINT('Origin',(16.1460502915689,23.7543320991532,35.0294657090004));
#37917=CARTESIAN_POINT('',(8.29725370442716,23.4543320991532,35.6713513169335));
#37918=CARTESIAN_POINT('Ctrl Pts',(8.29725370442717,23.4543320991532,35.6713513169335));
#37919=CARTESIAN_POINT('Ctrl Pts',(8.15831890747932,23.6006388275175,35.7674658348272));
#37920=CARTESIAN_POINT('Ctrl Pts',(8.01409135636202,23.7543320991532,35.8672418581646));
#37921=CARTESIAN_POINT('',(7.98602634532737,23.7543320991532,35.5240708007294));
#37922=CARTESIAN_POINT('Ctrl Pts',(7.98602634532737,23.7543320991532,35.5240708007294));
#37923=CARTESIAN_POINT('Ctrl Pts',(8.14454869178474,23.6006388275175,35.5990875122539));
#37924=CARTESIAN_POINT('Ctrl Pts',(8.29725370442716,23.4543320991532,35.6713513169335));
#37925=CARTESIAN_POINT('',(7.97286324518834,23.7543320991532,35.2016240804971));
#37926=CARTESIAN_POINT('Origin',(16.1460502915689,23.7543320991532,35.0294657090004));
#37927=CARTESIAN_POINT('',(8.27105029156894,23.4543320991532,35.0294657090004));
#37928=CARTESIAN_POINT('Ctrl Pts',(8.27105029156893,23.4543320991532,35.0294657090004));
#37929=CARTESIAN_POINT('Ctrl Pts',(8.12474356320462,23.6006388275175,35.1139359380058));
#37930=CARTESIAN_POINT('Ctrl Pts',(7.97286324518834,23.7543320991532,35.2016240804971));
#37931=CARTESIAN_POINT('',(7.97286324518834,23.7543320991532,34.8573073375037));
#37932=CARTESIAN_POINT('Ctrl Pts',(7.97286324518833,23.7543320991532,34.8573073375037));
#37933=CARTESIAN_POINT('Ctrl Pts',(8.12474356320462,23.6006388275175,34.944995479995));
#37934=CARTESIAN_POINT('Ctrl Pts',(8.27105029156893,23.4543320991532,35.0294657090004));
#37935=CARTESIAN_POINT('',(7.98602634532736,23.7543320991532,34.5348606172715));
#37936=CARTESIAN_POINT('Origin',(16.1460502915689,23.7543320991532,35.0294657090004));
#37937=CARTESIAN_POINT('',(8.29725370442715,23.4543320991532,34.3875801010673));
#37938=CARTESIAN_POINT('Ctrl Pts',(8.29725370442715,23.4543320991532,34.3875801010673));
#37939=CARTESIAN_POINT('Ctrl Pts',(8.14454869178473,23.6006388275175,34.4598439057469));
#37940=CARTESIAN_POINT('Ctrl Pts',(7.98602634532737,23.7543320991532,34.5348606172715));
#37941=CARTESIAN_POINT('',(8.01409135636201,23.7543320991532,34.1916895598362));
#37942=CARTESIAN_POINT('Ctrl Pts',(8.01409135636201,23.7543320991532,34.1916895598362));
#37943=CARTESIAN_POINT('Ctrl Pts',(8.1583189074793,23.6006388275175,34.2914655831736));
#37944=CARTESIAN_POINT('Ctrl Pts',(8.29725370442715,23.4543320991532,34.3875801010673));
#37945=CARTESIAN_POINT('',(8.05349305851944,23.7543320991532,33.8713886693271));
#37946=CARTESIAN_POINT('Origin',(16.1460502915689,23.7543320991532,35.0294657090004));
#37947=CARTESIAN_POINT('',(8.37568956361252,23.4543320991532,33.7499661359513));
#37948=CARTESIAN_POINT('Ctrl Pts',(8.37568956361251,23.4543320991532,33.7499661359513));
#37949=CARTESIAN_POINT('Ctrl Pts',(8.21760249335657,23.6006388275175,33.8095426126077));
#37950=CARTESIAN_POINT('Ctrl Pts',(8.05349305851945,23.7543320991532,33.8713886693271));
#37951=CARTESIAN_POINT('',(8.1094363125707,23.7543320991532,33.5316470442181));
#37952=CARTESIAN_POINT('Ctrl Pts',(8.1094363125707,23.7543320991532,33.5316470442181));
#37953=CARTESIAN_POINT('Ctrl Pts',(8.24505128623219,23.6006388275175,33.642846955428));
#37954=CARTESIAN_POINT('Ctrl Pts',(8.37568956361251,23.4543320991532,33.7499661359513));
#37955=CARTESIAN_POINT('',(8.17481440491951,23.7543320991532,33.2156235330125));
#37956=CARTESIAN_POINT('Origin',(16.1460502915689,23.7543320991532,35.0294657090004));
#37957=CARTESIAN_POINT('',(8.50583589142315,23.4543320991532,33.1208670293914));
#37958=CARTESIAN_POINT('Ctrl Pts',(8.50583589142315,23.4543320991532,33.1208670293914));
#37959=CARTESIAN_POINT('Ctrl Pts',(8.3434188069237,23.6006388275175,33.1673597064018));
#37960=CARTESIAN_POINT('Ctrl Pts',(8.17481440491951,23.7543320991532,33.2156235330125));
#37961=CARTESIAN_POINT('',(8.25826360886166,23.7543320991532,32.8815722646913));
#37962=CARTESIAN_POINT('Ctrl Pts',(8.25826360886166,23.7543320991532,32.8815722646913));
#37963=CARTESIAN_POINT('Ctrl Pts',(8.38436350979251,23.6006388275175,33.0034560467115));
#37964=CARTESIAN_POINT('Ctrl Pts',(8.50583589142315,23.4543320991532,33.1208670293914));
#37965=CARTESIAN_POINT('',(8.34918301098388,23.7543320991532,32.5719292171162));
#37966=CARTESIAN_POINT('Origin',(16.1460502915689,23.7543320991532,35.0294657090004));
#37967=CARTESIAN_POINT('',(8.68682658552011,23.4543320991532,32.5044693321477));
#37968=CARTESIAN_POINT('Ctrl Pts',(8.68682658552011,23.4543320991532,32.5044693321477));
#37969=CARTESIAN_POINT('Ctrl Pts',(8.52116034567756,23.6006388275175,32.5375688084173));
#37970=CARTESIAN_POINT('Ctrl Pts',(8.34918301098388,23.7543320991532,32.5719292171162));
#37971=CARTESIAN_POINT('',(8.45958282413283,23.7543320991532,32.245791361659));
#37972=CARTESIAN_POINT('Ctrl Pts',(8.45958282413283,23.7543320991532,32.245791361659));
#37973=CARTESIAN_POINT('Ctrl Pts',(8.57532847829738,23.6006388275175,32.3775478980294));
#37974=CARTESIAN_POINT('Ctrl Pts',(8.68682658552011,23.4543320991532,32.5044693321477));
#37975=CARTESIAN_POINT('',(8.57543848240798,23.7543320991532,31.9445894011085));
#37976=CARTESIAN_POINT('Origin',(16.1460502915689,23.7543320991532,35.0294657090004));
#37977=CARTESIAN_POINT('',(8.91745718269554,23.4543320991532,31.9048750691968));
#37978=CARTESIAN_POINT('Ctrl Pts',(8.91745718269554,23.4543320991532,31.9048750691968));
#37979=CARTESIAN_POINT('Ctrl Pts',(8.74964426900305,23.6006388275175,31.9243610731722));
#37980=CARTESIAN_POINT('Ctrl Pts',(8.57543848240798,23.7543320991532,31.9445894011085));
#37981=CARTESIAN_POINT('',(8.71205421222193,23.7543320991532,31.6285353521343));
#37982=CARTESIAN_POINT('Ctrl Pts',(8.71205421222193,23.7543320991532,31.6285353521343));
#37983=CARTESIAN_POINT('Ctrl Pts',(8.81667535138839,23.6006388275175,31.7692878248437));
#37984=CARTESIAN_POINT('Ctrl Pts',(8.91745718269554,23.4543320991532,31.9048750691968));
#37985=CARTESIAN_POINT('',(8.85207512635903,23.7543320991532,31.337778927961));
#37986=CARTESIAN_POINT('Origin',(16.1460502915689,23.7543320991532,35.0294657090004));
#37987=CARTESIAN_POINT('',(9.19619287437661,23.4543320991532,31.3260744414326));
#37988=CARTESIAN_POINT('Ctrl Pts',(9.19619287437661,23.4543320991532,31.3260744414326));
#37989=CARTESIAN_POINT('Ctrl Pts',(9.02735005408761,23.6006388275175,31.3318172969722));
#37990=CARTESIAN_POINT('Ctrl Pts',(8.85207512635904,23.7543320991532,31.3377789279609));
#37991=CARTESIAN_POINT('',(9.01399761769606,23.7543320991532,31.0339119730205));
#37992=CARTESIAN_POINT('Ctrl Pts',(9.01399761769606,23.7543320991532,31.0339119730205));
#37993=CARTESIAN_POINT('Ctrl Pts',(9.10679800544456,23.6006388275175,31.1827236975856));
#37994=CARTESIAN_POINT('Ctrl Pts',(9.1961928743766,23.4543320991532,31.3260744414326));
#37995=CARTESIAN_POINT('',(9.17725197161336,23.7543320991532,30.7555360212558));
#37996=CARTESIAN_POINT('Origin',(16.1460502915689,23.7543320991532,35.0294657090004));
#37997=CARTESIAN_POINT('',(9.52117872052333,23.4543320991532,30.7719192715376));
#37998=CARTESIAN_POINT('Ctrl Pts',(9.52117872052333,23.4543320991532,30.7719192715376));
#37999=CARTESIAN_POINT('Ctrl Pts',(9.35242961474975,23.6006388275175,30.7638807608853));
#38000=CARTESIAN_POINT('Ctrl Pts',(9.17725197161336,23.7543320991532,30.7555360212558));
#38001=CARTESIAN_POINT('',(9.36340365700895,23.7543320991532,30.4658783447997));
#38002=CARTESIAN_POINT('Ctrl Pts',(9.36340365700895,23.7543320991532,30.4658783447997));
#38003=CARTESIAN_POINT('Ctrl Pts',(9.44376572207002,23.6006388275175,30.6217590037456));
#38004=CARTESIAN_POINT('Ctrl Pts',(9.52117872052333,23.4543320991532,30.7719192715376));
#38005=CARTESIAN_POINT('',(9.54880501991619,23.7543320991532,30.2017354114738));
#38006=CARTESIAN_POINT('Origin',(16.1460502915689,23.7543320991532,35.0294657090004));
#38007=CARTESIAN_POINT('',(9.89025199394849,23.4543320991532,30.2460973707382));
#38008=CARTESIAN_POINT('Ctrl Pts',(9.89025199394849,23.4543320991532,30.2460973707382));
#38009=CARTESIAN_POINT('Ctrl Pts',(9.7227196001476,23.6006388275175,30.2243309888561));
#38010=CARTESIAN_POINT('Ctrl Pts',(9.5488050199162,23.7543320991532,30.2017354114738));
#38011=CARTESIAN_POINT('',(9.75794709061692,23.7543320991532,29.9282146375487));
#38012=CARTESIAN_POINT('Ctrl Pts',(9.75794709061692,23.7543320991532,29.9282146375487));
#38013=CARTESIAN_POINT('Ctrl Pts',(9.82533603670636,23.6006388275175,30.0901268708088));
#38014=CARTESIAN_POINT('Ctrl Pts',(9.89025199394849,23.4543320991532,30.2460973707382));
#38015=CARTESIAN_POINT('',(9.96426164703304,23.7543320991532,29.6800625503025));
#38016=CARTESIAN_POINT('Origin',(16.1460502915689,23.7543320991532,35.0294657090004));
#38017=CARTESIAN_POINT('',(10.3009565729102,23.4543320991532,29.7521079970296));
#38018=CARTESIAN_POINT('Ctrl Pts',(10.3009565729102,23.4543320991532,29.7521079970297));
#38019=CARTESIAN_POINT('Ctrl Pts',(10.1357557915219,23.6006388275175,29.7167585955981));
#38020=CARTESIAN_POINT('Ctrl Pts',(9.96426164703304,23.7543320991532,29.6800625503025));
#38021=CARTESIAN_POINT('',(10.1950022970644,23.7543320991532,29.4244989145311));
#38022=CARTESIAN_POINT('Ctrl Pts',(10.1950022970644,23.7543320991532,29.4244989145311));
#38023=CARTESIAN_POINT('Ctrl Pts',(10.2489696618644,23.6006388275175,29.5913652229065));
#38024=CARTESIAN_POINT('Ctrl Pts',(10.3009565729102,23.4543320991532,29.7521079970296));
#38025=CARTESIAN_POINT('',(10.4208570576559,23.7543320991532,29.1939890845628));
#38026=CARTESIAN_POINT('Origin',(16.1460502915689,23.7543320991532,35.0294657090004));
#38027=CARTESIAN_POINT('',(10.7505592861971,23.4543320991532,29.2932385681916));
#38028=CARTESIAN_POINT('Ctrl Pts',(10.7505592861971,23.4543320991532,29.2932385681915));
#38029=CARTESIAN_POINT('Ctrl Pts',(10.5887895011652,23.6006388275175,29.2445413916448));
#38030=CARTESIAN_POINT('Ctrl Pts',(10.4208570576559,23.7543320991532,29.1939890845628));
#38031=CARTESIAN_POINT('',(10.6716607460615,23.7543320991532,28.9580833207762));
#38032=CARTESIAN_POINT('Ctrl Pts',(10.6716607460615,23.7543320991532,28.9580833207762));
#38033=CARTESIAN_POINT('Ctrl Pts',(10.7118473856633,23.6006388275175,29.1287932365158));
#38034=CARTESIAN_POINT('Ctrl Pts',(10.7505592861971,23.4543320991532,29.2932385681916));
#38035=CARTESIAN_POINT('',(10.9155526846601,23.7543320991532,28.746749752973));
#38036=CARTESIAN_POINT('Origin',(16.1460502915689,23.7543320991532,35.0294657090004));
#38037=CARTESIAN_POINT('',(11.2360681019313,23.4543320991532,28.8725427845647));
#38038=CARTESIAN_POINT('Ctrl Pts',(11.2360681019313,23.4543320991532,28.8725427845647));
#38039=CARTESIAN_POINT('Ctrl Pts',(11.0788058644852,23.6006388275175,28.8108219045781));
#38040=CARTESIAN_POINT('Ctrl Pts',(10.9155526846601,23.7543320991532,28.746749752973));
#38041=CARTESIAN_POINT('',(11.1847503542732,23.7543320991532,28.5320717751074));
#38042=CARTESIAN_POINT('Ctrl Pts',(11.1847503542732,23.7543320991532,28.5320717751074));
#38043=CARTESIAN_POINT('Ctrl Pts',(11.2108888332206,23.6006388275175,28.705489251887));
#38044=CARTESIAN_POINT('Ctrl Pts',(11.2360681019313,23.4543320991532,28.8725427845647));
#38045=CARTESIAN_POINT('',(11.4450564102669,23.7543320991532,28.3413208594953));
#38046=CARTESIAN_POINT('Origin',(16.1460502915689,23.7543320991532,35.0294657090004));
#38047=CARTESIAN_POINT('',(11.7542520390476,23.4543320991532,28.4928203071792));
#38048=CARTESIAN_POINT('Ctrl Pts',(11.7542520390476,23.4543320991532,28.4928203071792));
#38049=CARTESIAN_POINT('Ctrl Pts',(11.6025439034309,23.6006388275175,28.4184864660259));
#38050=CARTESIAN_POINT('Ctrl Pts',(11.4450564102669,23.7543320991532,28.3413208594953));
#38051=CARTESIAN_POINT('',(11.7308565950108,23.7543320991532,28.1492993140741));
#38052=CARTESIAN_POINT('Ctrl Pts',(11.7308565950108,23.7543320991532,28.1492993140741));
#38053=CARTESIAN_POINT('Ctrl Pts',(11.7427729660389,23.6006388275175,28.3242702871977));
#38054=CARTESIAN_POINT('Ctrl Pts',(11.7542520390476,23.4543320991532,28.4928203071792));
#38055=CARTESIAN_POINT('',(12.0058444745444,23.7543320991532,27.9804004665249));
#38056=CARTESIAN_POINT('Origin',(16.1460502915689,23.7543320991532,35.0294657090004));
#38057=CARTESIAN_POINT('',(12.3016626689386,23.4543320991532,28.1565981264722));
#38058=CARTESIAN_POINT('Ctrl Pts',(12.3016626689386,23.4543320991532,28.1565981264722));
#38059=CARTESIAN_POINT('Ctrl Pts',(12.1565182277639,23.6006388275175,28.0701460036008));
#38060=CARTESIAN_POINT('Ctrl Pts',(12.0058444745444,23.7543320991532,27.9804004665249));
#38061=CARTESIAN_POINT('',(12.3063452213432,23.7543320991532,27.8123132252514));
#38062=CARTESIAN_POINT('Ctrl Pts',(12.3063452213432,23.7543320991532,27.8123132252514));
#38063=CARTESIAN_POINT('Ctrl Pts',(12.3039601829689,23.6006388275175,27.9876732917611));
#38064=CARTESIAN_POINT('Ctrl Pts',(12.3016626689386,23.4543320991532,28.1565981264722));
#38065=CARTESIAN_POINT('',(12.5941849254483,23.7543320991532,27.6663904397292));
#38066=CARTESIAN_POINT('Origin',(16.1460502915689,23.7543320991532,35.0294657090004));
#38067=CARTESIAN_POINT('',(12.874657064179,23.4543320991532,27.8661137455836));
#38068=CARTESIAN_POINT('Ctrl Pts',(12.874657064179,23.4543320991532,27.8661137455836));
#38069=CARTESIAN_POINT('Ctrl Pts',(12.7370422297551,23.6006388275175,27.7681186656083));
#38070=CARTESIAN_POINT('Ctrl Pts',(12.5941849254483,23.7543320991532,27.6663904397292));
#38071=CARTESIAN_POINT('',(12.9073864514113,23.7543320991532,27.5233560954618));
#38072=CARTESIAN_POINT('Ctrl Pts',(12.9073864514113,23.7543320991532,27.5233560954618));
#38073=CARTESIAN_POINT('Ctrl Pts',(12.8907158756715,23.6006388275175,27.6979382630472));
#38074=CARTESIAN_POINT('Ctrl Pts',(12.874657064179,23.4543320991532,27.8661137455836));
#38075=CARTESIAN_POINT('',(13.2061624543472,23.7543320991532,27.4013804640286));
#38076=CARTESIAN_POINT('Origin',(16.1460502915689,23.7543320991532,35.0294657090004));
#38077=CARTESIAN_POINT('',(13.4694220416057,23.4543320991532,27.6233002901416));
#38078=CARTESIAN_POINT('Ctrl Pts',(13.4694220416057,23.4543320991532,27.6233002901416));
#38079=CARTESIAN_POINT('Ctrl Pts',(13.3402526179508,23.6006388275175,27.5144143941516));
#38080=CARTESIAN_POINT('Ctrl Pts',(13.2061624543472,23.7543320991532,27.4013804640286));
#38081=CARTESIAN_POINT('',(13.5299804549937,23.7543320991532,27.2843508867294));
#38082=CARTESIAN_POINT('Ctrl Pts',(13.5299804549937,23.7543320991532,27.2843508867294));
#38083=CARTESIAN_POINT('Ctrl Pts',(13.4991352818195,23.6006388275175,27.4569933398693));
#38084=CARTESIAN_POINT('Ctrl Pts',(13.4694220416057,23.4543320991532,27.6233002901416));
#38085=CARTESIAN_POINT('',(13.8377044517554,23.7543320991532,27.1871341370879));
#38086=CARTESIAN_POINT('Origin',(16.1460502915689,23.7543320991532,35.0294657090004));
#38087=CARTESIAN_POINT('',(14.0819995384234,23.4543320991532,27.4297736436309));
#38088=CARTESIAN_POINT('Ctrl Pts',(14.0819995384234,23.4543320991532,27.4297736436309));
#38089=CARTESIAN_POINT('Ctrl Pts',(13.9621351267405,23.6006388275175,27.310721549299));
#38090=CARTESIAN_POINT('Ctrl Pts',(13.8377044517554,23.7543320991532,27.1871341370879));
#38091=CARTESIAN_POINT('',(14.1699839717174,23.7543320991532,27.0968881392852));
#38092=CARTESIAN_POINT('Ctrl Pts',(14.1699839717174,23.7543320991532,27.0968881392852));
#38093=CARTESIAN_POINT('Ctrl Pts',(14.1251694706471,23.6006388275175,27.2664419709379));
#38094=CARTESIAN_POINT('Ctrl Pts',(14.0819995384234,23.4543320991532,27.4297736436309));
#38095=CARTESIAN_POINT('',(14.4846081098774,23.7543320991532,27.0250772328645));
#38096=CARTESIAN_POINT('Origin',(16.1460502915689,23.7543320991532,35.0294657090004));
#38097=CARTESIAN_POINT('',(14.7083129524589,23.4543320991532,27.2868216939543));
#38098=CARTESIAN_POINT('Ctrl Pts',(14.7083129524589,23.4543320991532,27.2868216939543));
#38099=CARTESIAN_POINT('Ctrl Pts',(14.5985512306315,23.6006388275175,27.1583956733261));
#38100=CARTESIAN_POINT('Ctrl Pts',(14.4846081098774,23.7543320991532,27.0250772328645));
#38101=CARTESIAN_POINT('',(14.8231378837717,23.7543320991532,26.9622153867842));
#38102=CARTESIAN_POINT('Ctrl Pts',(14.8231378837717,23.7543320991532,26.9622153867842));
#38103=CARTESIAN_POINT('Ctrl Pts',(14.7646522879161,23.6006388275175,27.1275522441746));
#38104=CARTESIAN_POINT('Ctrl Pts',(14.7083129524589,23.4543320991532,27.2868216939543));
#38105=CARTESIAN_POINT('',(15.1425683915998,23.7543320991532,26.9162882133188));
#38106=CARTESIAN_POINT('Origin',(16.1460502915689,23.7543320991532,35.0294657090004));
#38107=CARTESIAN_POINT('',(15.3441942712762,23.4543320991532,27.1953957627515));
#38108=CARTESIAN_POINT('Ctrl Pts',(15.3441942712762,23.4543320991532,27.1953957627515));
#38109=CARTESIAN_POINT('Ctrl Pts',(15.2452656854537,23.6006388275175,27.0584504698055));
#38110=CARTESIAN_POINT('Ctrl Pts',(15.1425683915998,23.7543320991532,26.9162882133188));
#38111=CARTESIAN_POINT('',(15.4850955596347,23.7543320991532,26.881228854175));
#38112=CARTESIAN_POINT('Ctrl Pts',(15.4850955596347,23.7543320991532,26.881228854175));
#38113=CARTESIAN_POINT('Ctrl Pts',(15.4133280809848,23.6006388275175,27.0412484477957));
#38114=CARTESIAN_POINT('Ctrl Pts',(15.3441942712762,23.4543320991532,27.1953957627515));
#38115=CARTESIAN_POINT('',(15.8072066798037,23.7543320991532,26.8614910514267));
#38116=CARTESIAN_POINT('Origin',(16.1460502915689,23.7543320991532,35.0294657090004));
#38117=CARTESIAN_POINT('Ctrl Pts',(15.9854118096115,23.4543320991532,27.1561042745104));
#38118=CARTESIAN_POINT('Ctrl Pts',(15.8979747132105,23.6006388275175,27.0115510575768));
#38119=CARTESIAN_POINT('Ctrl Pts',(15.8072066798037,23.7543320991532,26.8614910514267));
#38120=CARTESIAN_POINT('Origin',(16.1460502915689,-2.04566790084674,35.0294657090004));
#38121=CARTESIAN_POINT('',(16.1460502915689,32.8543320991532,33.0294657090004));
#38122=CARTESIAN_POINT('Origin',(16.1460502915689,32.8543320991532,35.0294657090004));
#38123=CARTESIAN_POINT('',(16.1460502915689,-2.04566790084674,33.0294657090004));
#38124=CARTESIAN_POINT('Origin',(16.1460502915689,-2.04566790084674,35.0294657090004));
#38125=CARTESIAN_POINT('',(8.05349305851946,42.8553320991532,36.1875427486737));
#38126=CARTESIAN_POINT('',(8.01409135636202,42.8553320991532,35.8672418581646));
#38127=CARTESIAN_POINT('Origin',(16.1460502915689,-2.04566790084674,35.0294657090004));
#38128=CARTESIAN_POINT('',(8.10943631257073,42.8553320991532,36.5272843737828));
#38129=CARTESIAN_POINT('',(8.17481440491953,42.8553320991532,36.8433078849883));
#38130=CARTESIAN_POINT('Origin',(16.1460502915689,-2.04566790084674,35.0294657090004));
#38131=CARTESIAN_POINT('',(8.25826360886169,42.8553320991532,37.1773591533095));
#38132=CARTESIAN_POINT('',(8.34918301098391,42.8553320991532,37.4870022008846));
#38133=CARTESIAN_POINT('Origin',(16.1460502915689,-2.04566790084674,35.0294657090004));
#38134=CARTESIAN_POINT('',(8.45958282413287,42.8553320991532,37.8131400563419));
#38135=CARTESIAN_POINT('',(8.57543848240802,42.8553320991532,38.1143420168924));
#38136=CARTESIAN_POINT('Origin',(16.1460502915689,-2.04566790084674,35.0294657090004));
#38137=CARTESIAN_POINT('',(8.71205421222198,42.8553320991532,38.4303960658666));
#38138=CARTESIAN_POINT('',(8.85207512635908,42.8553320991532,38.7211524900399));
#38139=CARTESIAN_POINT('Origin',(16.1460502915689,-2.04566790084674,35.0294657090004));
#38140=CARTESIAN_POINT('',(9.01399761769612,42.8553320991532,39.0250194449803));
#38141=CARTESIAN_POINT('',(9.17725197161342,42.8553320991532,39.303395396745));
#38142=CARTESIAN_POINT('Origin',(16.1460502915689,-2.04566790084674,35.0294657090004));
#38143=CARTESIAN_POINT('',(9.36340365700902,42.8553320991532,39.5930530732011));
#38144=CARTESIAN_POINT('',(9.54880501991626,42.8553320991532,39.857196006527));
#38145=CARTESIAN_POINT('Origin',(16.1460502915689,-2.04566790084674,35.0294657090004));
#38146=CARTESIAN_POINT('',(9.75794709061699,42.8553320991532,40.1307167804521));
#38147=CARTESIAN_POINT('',(9.96426164703311,42.8553320991532,40.3788688676983));
#38148=CARTESIAN_POINT('Origin',(16.1460502915689,-2.04566790084674,35.0294657090004));
#38149=CARTESIAN_POINT('',(10.1950022970645,42.8553320991532,40.6344325034697));
#38150=CARTESIAN_POINT('',(10.420857057656,42.8553320991532,40.864942333438));
#38151=CARTESIAN_POINT('Origin',(16.1460502915689,-2.04566790084674,35.0294657090004));
#38152=CARTESIAN_POINT('',(10.6716607460615,42.8553320991532,41.1008480972246));
#38153=CARTESIAN_POINT('',(10.9155526846602,42.8553320991532,41.3121816650278));
#38154=CARTESIAN_POINT('Origin',(16.1460502915689,-2.04566790084674,35.0294657090004));
#38155=CARTESIAN_POINT('',(11.1847503542733,42.8553320991532,41.5268596428934));
#38156=CARTESIAN_POINT('',(11.445056410267,42.8553320991532,41.7176105585055));
#38157=CARTESIAN_POINT('Origin',(16.1460502915689,-2.04566790084674,35.0294657090004));
#38158=CARTESIAN_POINT('',(11.7308565950109,42.8553320991532,41.9096321039267));
#38159=CARTESIAN_POINT('',(12.0058444745445,42.8553320991532,42.0785309514759));
#38160=CARTESIAN_POINT('Origin',(16.1460502915689,-2.04566790084674,35.0294657090004));
#38161=CARTESIAN_POINT('',(12.3063452213433,42.8553320991532,42.2466181927493));
#38162=CARTESIAN_POINT('',(12.5941849254484,42.8553320991532,42.3925409782716));
#38163=CARTESIAN_POINT('Origin',(16.1460502915689,-2.04566790084674,35.0294657090004));
#38164=CARTESIAN_POINT('',(12.9073864514114,42.8553320991532,42.5355753225389));
#38165=CARTESIAN_POINT('',(13.2061624543473,42.8553320991532,42.6575509539721));
#38166=CARTESIAN_POINT('Origin',(16.1460502915689,-2.04566790084674,35.0294657090004));
#38167=CARTESIAN_POINT('',(13.5299804549939,42.8553320991532,42.7745805312714));
#38168=CARTESIAN_POINT('',(13.8377044517555,42.8553320991532,42.8717972809129));
#38169=CARTESIAN_POINT('Origin',(16.1460502915689,-2.04566790084674,35.0294657090004));
#38170=CARTESIAN_POINT('',(14.1699839717175,42.8553320991532,42.9620432787156));
#38171=CARTESIAN_POINT('',(14.4846081098775,42.8553320991532,43.0338541851362));
#38172=CARTESIAN_POINT('Origin',(16.1460502915689,-2.04566790084674,35.0294657090004));
#38173=CARTESIAN_POINT('',(14.8231378837718,42.8553320991532,43.0967160312165));
#38174=CARTESIAN_POINT('',(15.1425683915999,42.8553320991532,43.142643204682));
#38175=CARTESIAN_POINT('Origin',(16.1460502915689,-2.04566790084674,35.0294657090004));
#38176=CARTESIAN_POINT('',(15.4850955596348,42.8553320991532,43.1777025638257));
#38177=CARTESIAN_POINT('',(15.8072066798038,42.8553320991532,43.197440366574));
#38178=CARTESIAN_POINT('Origin',(16.1460502915689,-2.04566790084674,35.0294657090004));
#38179=CARTESIAN_POINT('',(16.151451780189,42.8553320991532,43.2044639245305));
#38180=CARTESIAN_POINT('',(16.4740999163387,42.8553320991532,43.1978810047409));
#38181=CARTESIAN_POINT('Origin',(16.1460502915689,-2.04566790084674,35.0294657090004));
#38182=CARTESIAN_POINT('',(16.8177720547276,42.8553320991532,43.1768220208907));
#38183=CARTESIAN_POINT('',(17.1388100367452,42.8553320991532,43.1439621868083));
#38184=CARTESIAN_POINT('Origin',(16.1460502915689,-2.04566790084674,35.0294657090004));
#38185=CARTESIAN_POINT('',(17.4796221317587,42.8553320991532,43.0949608052144));
#38186=CARTESIAN_POINT('',(17.7969135048413,42.8553320991532,43.0360427336136));
#38187=CARTESIAN_POINT('Origin',(16.1460502915689,-2.04566790084674,35.0294657090004));
#38188=CARTESIAN_POINT('',(18.1325975082171,42.8553320991532,42.9594250503859));
#38189=CARTESIAN_POINT('',(18.4440307506264,42.8553320991532,42.8748408313122));
#38190=CARTESIAN_POINT('Origin',(16.1460502915689,-2.04566790084674,35.0294657090004));
#38191=CARTESIAN_POINT('',(18.772352740706,42.8553320991532,42.7711167244916));
#38192=CARTESIAN_POINT('',(19.0758553155965,42.8553320991532,42.6614292519677));
#38193=CARTESIAN_POINT('Origin',(16.1460502915689,-2.04566790084674,35.0294657090004));
#38194=CARTESIAN_POINT('',(19.3946303637053,42.8553320991532,42.5312889883718));
#38195=CARTESIAN_POINT('',(19.6881825115155,42.8553320991532,42.3972282144301));
#38196=CARTESIAN_POINT('Origin',(16.1460502915689,-2.04566790084674,35.0294657090004));
#38197=CARTESIAN_POINT('',(19.9952892223025,42.8553320991532,42.2415378560414));
#38198=CARTESIAN_POINT('',(20.2769374019215,42.8553320991532,42.0839959330141));
#38199=CARTESIAN_POINT('Origin',(16.1460502915689,-2.04566790084674,35.0294657090004));
#38200=CARTESIAN_POINT('',(20.5703320308954,42.8553320991532,41.9037915734806));
#38201=CARTESIAN_POINT('',(20.8382019201565,42.8553320991532,41.7238169168728));
#38202=CARTESIAN_POINT('Origin',(16.1460502915689,-2.04566790084674,35.0294657090004));
#38203=CARTESIAN_POINT('',(21.1159319744682,42.8553320991532,41.5202977864757));
#38204=CARTESIAN_POINT('',(21.3682409434537,42.8553320991532,41.3190880979334));
#38205=CARTESIAN_POINT('Origin',(16.1460502915689,-2.04566790084674,35.0294657090004));
#38206=CARTESIAN_POINT('',(21.628458175414,42.8553320991532,41.0936085829071));
#38207=CARTESIAN_POINT('',(21.8635271495635,42.8553320991532,40.8725028797102));
#38208=CARTESIAN_POINT('Origin',(16.1460502915689,-2.04566790084674,35.0294657090004));
#38209=CARTESIAN_POINT('',(22.1044998564265,42.8553320991532,40.6265635090257));
#38210=CARTESIAN_POINT('',(22.3207644905006,42.8553320991532,40.3870332131493));
#38211=CARTESIAN_POINT('Origin',(16.1460502915689,-2.04566790084674,35.0294657090004));
#38212=CARTESIAN_POINT('',(22.5408890386598,42.8553320991532,40.1222706727414));
#38213=CARTESIAN_POINT('',(22.7369101271999,42.8553320991532,39.8659098187846));
#38214=CARTESIAN_POINT('Origin',(16.1460502915689,-2.04566790084674,35.0294657090004));
#38215=CARTESIAN_POINT('',(22.9347216241054,42.8553320991532,39.584086059677));
#38216=CARTESIAN_POINT('',(23.1091946791084,42.8553320991532,39.3126006868265));
#38217=CARTESIAN_POINT('Origin',(16.1460502915689,-2.04566790084674,35.0294657090004));
#38218=CARTESIAN_POINT('',(23.2833767218849,42.8553320991532,39.0155911996383));
#38219=CARTESIAN_POINT('',(23.4351406539558,42.8553320991532,38.7307879982584));
#38220=CARTESIAN_POINT('Origin',(16.1460502915689,-2.04566790084674,35.0294657090004));
#38221=CARTESIAN_POINT('',(23.5845340898466,42.8553320991532,38.4205693321238));
#38222=CARTESIAN_POINT('',(23.7125789350568,42.8553320991532,38.1243436205306));
#38223=CARTESIAN_POINT('Origin',(16.1460502915689,-2.04566790084674,35.0294657090004));
#38224=CARTESIAN_POINT('',(23.8361895753942,42.8553320991532,37.8029802294902));
#38225=CARTESIAN_POINT('',(23.9396632164247,42.8553320991532,37.4973033409204));
#38226=CARTESIAN_POINT('Origin',(16.1460502915689,-2.04566790084674,35.0294657090004));
#38227=CARTESIAN_POINT('',(24.0366684527916,42.8553320991532,37.1669338453204));
#38228=CARTESIAN_POINT('',(24.1148822896334,42.8553320991532,36.8538400090343));
#38229=CARTESIAN_POINT('Origin',(16.1460502915689,-2.04566790084674,35.0294657090004));
#38230=CARTESIAN_POINT('',(24.1846365681864,42.8553320991532,36.5166629633608));
#38231=CARTESIAN_POINT('',(24.2370701006596,42.8553320991532,36.1982357671821));
#38232=CARTESIAN_POINT('Origin',(16.1460502915689,-2.04566790084674,35.0294657090004));
#38233=CARTESIAN_POINT('',(24.2791092181837,42.8553320991532,35.8564950290437));
#38234=CARTESIAN_POINT('',(24.3054135097807,42.8553320991532,35.5348535534261));
#38235=CARTESIAN_POINT('Origin',(16.1460502915689,-2.04566790084674,35.0294657090004));
#38236=CARTESIAN_POINT('',(24.3194577028847,42.8553320991532,35.1908233510519));
#38237=CARTESIAN_POINT('',(24.3194577028847,42.8553320991532,34.8681080669487));
#38238=CARTESIAN_POINT('Origin',(16.1460502915689,-2.04566790084674,35.0294657090004));
#38239=CARTESIAN_POINT('',(24.3054135097807,42.8553320991532,34.5240778645745));
#38240=CARTESIAN_POINT('',(24.2791092181837,42.8553320991532,34.2024363889569));
#38241=CARTESIAN_POINT('Origin',(16.1460502915689,-2.04566790084674,35.0294657090004));
#38242=CARTESIAN_POINT('',(24.2370701006596,42.8553320991532,33.8606956508185));
#38243=CARTESIAN_POINT('',(24.1846365681864,42.8553320991532,33.5422684546398));
#38244=CARTESIAN_POINT('Origin',(16.1460502915689,-2.04566790084674,35.0294657090004));
#38245=CARTESIAN_POINT('',(24.1148822896334,42.8553320991532,33.2050914089663));
#38246=CARTESIAN_POINT('',(24.0366684527916,42.8553320991532,32.8919975726802));
#38247=CARTESIAN_POINT('Origin',(16.1460502915689,-2.04566790084674,35.0294657090004));
#38248=CARTESIAN_POINT('',(23.9396632164247,42.8553320991532,32.5616280770803));
#38249=CARTESIAN_POINT('',(23.8361895753941,42.8553320991532,32.2559511885104));
#38250=CARTESIAN_POINT('Origin',(16.1460502915689,-2.04566790084674,35.0294657090004));
#38251=CARTESIAN_POINT('',(23.7125789350568,42.8553320991532,31.9345877974701));
#38252=CARTESIAN_POINT('',(23.5845340898465,42.8553320991532,31.6383620858768));
#38253=CARTESIAN_POINT('Origin',(16.1460502915689,-2.04566790084674,35.0294657090004));
#38254=CARTESIAN_POINT('',(23.4351406539558,42.8553320991532,31.3281434197422));
#38255=CARTESIAN_POINT('',(23.2833767218848,42.8553320991532,31.0433402183623));
#38256=CARTESIAN_POINT('Origin',(16.1460502915689,-2.04566790084674,35.0294657090004));
#38257=CARTESIAN_POINT('',(23.1091946791084,42.8553320991532,30.7463307311742));
#38258=CARTESIAN_POINT('',(22.9347216241054,42.8553320991532,30.4748453583237));
#38259=CARTESIAN_POINT('Origin',(16.1460502915689,-2.04566790084674,35.0294657090004));
#38260=CARTESIAN_POINT('',(22.7369101271998,42.8553320991532,30.193021599216));
#38261=CARTESIAN_POINT('',(22.5408890386598,42.8553320991532,29.9366607452593));
#38262=CARTESIAN_POINT('Origin',(16.1460502915689,-2.04566790084674,35.0294657090004));
#38263=CARTESIAN_POINT('',(22.3207644905005,42.8553320991532,29.6718982048514));
#38264=CARTESIAN_POINT('',(22.1044998564264,42.8553320991532,29.4323679089749));
#38265=CARTESIAN_POINT('Origin',(16.1460502915689,-2.04566790084674,35.0294657090004));
#38266=CARTESIAN_POINT('',(21.8635271495634,42.8553320991532,29.1864285382904));
#38267=CARTESIAN_POINT('',(21.6284581754139,42.8553320991532,28.9653228350936));
#38268=CARTESIAN_POINT('Origin',(16.1460502915689,-2.04566790084674,35.0294657090004));
#38269=CARTESIAN_POINT('',(21.3682409434536,42.8553320991532,28.7398433200673));
#38270=CARTESIAN_POINT('',(21.1159319744681,42.8553320991532,28.538633631525));
#38271=CARTESIAN_POINT('Origin',(16.1460502915689,-2.04566790084674,35.0294657090004));
#38272=CARTESIAN_POINT('',(20.8382019201564,42.8553320991532,28.3351145011278));
#38273=CARTESIAN_POINT('',(20.5703320308953,42.8553320991532,28.15513984452));
#38274=CARTESIAN_POINT('Origin',(16.1460502915689,-2.04566790084674,35.0294657090004));
#38275=CARTESIAN_POINT('',(20.2769374019214,42.8553320991532,27.9749354849866));
#38276=CARTESIAN_POINT('',(19.9952892223024,42.8553320991532,27.8173935619593));
#38277=CARTESIAN_POINT('Origin',(16.1460502915689,-2.04566790084674,35.0294657090004));
#38278=CARTESIAN_POINT('',(19.6881825115154,42.8553320991532,27.6617032035706));
#38279=CARTESIAN_POINT('',(19.3946303637052,42.8553320991532,27.5276424296289));
#38280=CARTESIAN_POINT('Origin',(16.1460502915689,-2.04566790084674,35.0294657090004));
#38281=CARTESIAN_POINT('',(19.0758553155964,42.8553320991532,27.397502166033));
#38282=CARTESIAN_POINT('',(18.7723527407059,42.8553320991532,27.2878146935091));
#38283=CARTESIAN_POINT('Origin',(16.1460502915689,-2.04566790084674,35.0294657090004));
#38284=CARTESIAN_POINT('',(18.4440307506263,42.8553320991532,27.1840905866885));
#38285=CARTESIAN_POINT('',(18.132597508217,42.8553320991532,27.0995063676148));
#38286=CARTESIAN_POINT('Origin',(16.1460502915689,-2.04566790084674,35.0294657090004));
#38287=CARTESIAN_POINT('',(17.7969135048412,42.8553320991532,27.0228886843871));
#38288=CARTESIAN_POINT('',(17.4796221317586,42.8553320991532,26.9639706127863));
#38289=CARTESIAN_POINT('Origin',(16.1460502915689,-2.04566790084674,35.0294657090004));
#38290=CARTESIAN_POINT('',(17.1388100367451,42.8553320991532,26.9149692311924));
#38291=CARTESIAN_POINT('',(16.8177720547275,42.8553320991532,26.88210939711));
#38292=CARTESIAN_POINT('Origin',(16.1460502915689,-2.04566790084674,35.0294657090004));
#38293=CARTESIAN_POINT('',(16.4740999163386,42.8553320991532,26.8610504132598));
#38294=CARTESIAN_POINT('',(16.1514517801889,42.8553320991532,26.8544674934702));
#38295=CARTESIAN_POINT('Origin',(16.1460502915689,-2.04566790084674,35.0294657090004));
#38296=CARTESIAN_POINT('',(15.8072066798037,42.8553320991532,26.8614910514267));
#38297=CARTESIAN_POINT('',(15.4850955596347,42.8553320991532,26.881228854175));
#38298=CARTESIAN_POINT('Origin',(16.1460502915689,-2.04566790084674,35.0294657090004));
#38299=CARTESIAN_POINT('',(15.1425683915998,42.8553320991532,26.9162882133188));
#38300=CARTESIAN_POINT('',(14.8231378837717,42.8553320991532,26.9622153867842));
#38301=CARTESIAN_POINT('Origin',(16.1460502915689,-2.04566790084674,35.0294657090004));
#38302=CARTESIAN_POINT('',(14.4846081098774,42.8553320991532,27.0250772328645));
#38303=CARTESIAN_POINT('',(14.1699839717174,42.8553320991532,27.0968881392852));
#38304=CARTESIAN_POINT('Origin',(16.1460502915689,-2.04566790084674,35.0294657090004));
#38305=CARTESIAN_POINT('',(13.8377044517554,42.8553320991532,27.1871341370879));
#38306=CARTESIAN_POINT('',(13.5299804549937,42.8553320991532,27.2843508867294));
#38307=CARTESIAN_POINT('Origin',(16.1460502915689,-2.04566790084674,35.0294657090004));
#38308=CARTESIAN_POINT('',(13.2061624543472,42.8553320991532,27.4013804640286));
#38309=CARTESIAN_POINT('',(12.9073864514113,42.8553320991532,27.5233560954618));
#38310=CARTESIAN_POINT('Origin',(16.1460502915689,-2.04566790084674,35.0294657090004));
#38311=CARTESIAN_POINT('',(12.5941849254483,42.8553320991532,27.6663904397292));
#38312=CARTESIAN_POINT('',(12.3063452213433,42.8553320991532,27.8123132252514));
#38313=CARTESIAN_POINT('Origin',(16.1460502915689,-2.04566790084674,35.0294657090004));
#38314=CARTESIAN_POINT('',(12.0058444745444,42.8553320991532,27.9804004665249));
#38315=CARTESIAN_POINT('',(11.7308565950108,42.8553320991532,28.1492993140741));
#38316=CARTESIAN_POINT('Origin',(16.1460502915689,-2.04566790084674,35.0294657090004));
#38317=CARTESIAN_POINT('',(11.4450564102669,42.8553320991532,28.3413208594953));
#38318=CARTESIAN_POINT('',(11.1847503542732,42.8553320991532,28.5320717751074));
#38319=CARTESIAN_POINT('Origin',(16.1460502915689,-2.04566790084674,35.0294657090004));
#38320=CARTESIAN_POINT('',(10.9155526846601,42.8553320991532,28.746749752973));
#38321=CARTESIAN_POINT('',(10.6716607460615,42.8553320991532,28.9580833207762));
#38322=CARTESIAN_POINT('Origin',(16.1460502915689,-2.04566790084674,35.0294657090004));
#38323=CARTESIAN_POINT('',(10.4208570576559,42.8553320991532,29.1939890845628));
#38324=CARTESIAN_POINT('',(10.1950022970644,42.8553320991532,29.4244989145311));
#38325=CARTESIAN_POINT('Origin',(16.1460502915689,-2.04566790084674,35.0294657090004));
#38326=CARTESIAN_POINT('',(9.96426164703304,42.8553320991532,29.6800625503025));
#38327=CARTESIAN_POINT('',(9.75794709061692,42.8553320991532,29.9282146375487));
#38328=CARTESIAN_POINT('Origin',(16.1460502915689,-2.04566790084674,35.0294657090004));
#38329=CARTESIAN_POINT('',(9.5488050199162,42.8553320991532,30.2017354114738));
#38330=CARTESIAN_POINT('',(9.36340365700895,42.8553320991532,30.4658783447997));
#38331=CARTESIAN_POINT('Origin',(16.1460502915689,-2.04566790084674,35.0294657090004));
#38332=CARTESIAN_POINT('',(9.17725197161336,42.8553320991532,30.7555360212558));
#38333=CARTESIAN_POINT('',(9.01399761769606,42.8553320991532,31.0339119730205));
#38334=CARTESIAN_POINT('Origin',(16.1460502915689,-2.04566790084674,35.0294657090004));
#38335=CARTESIAN_POINT('',(8.85207512635903,42.8553320991532,31.337778927961));
#38336=CARTESIAN_POINT('',(8.71205421222193,42.8553320991532,31.6285353521343));
#38337=CARTESIAN_POINT('Origin',(16.1460502915689,-2.04566790084674,35.0294657090004));
#38338=CARTESIAN_POINT('',(8.57543848240798,42.8553320991532,31.9445894011085));
#38339=CARTESIAN_POINT('',(8.45958282413283,42.8553320991532,32.245791361659));
#38340=CARTESIAN_POINT('Origin',(16.1460502915689,-2.04566790084674,35.0294657090004));
#38341=CARTESIAN_POINT('',(8.34918301098387,42.8553320991532,32.5719292171162));
#38342=CARTESIAN_POINT('',(8.25826360886166,42.8553320991532,32.8815722646913));
#38343=CARTESIAN_POINT('Origin',(16.1460502915689,-2.04566790084674,35.0294657090004));
#38344=CARTESIAN_POINT('',(8.17481440491951,42.8553320991532,33.2156235330125));
#38345=CARTESIAN_POINT('',(8.1094363125707,42.8553320991532,33.5316470442181));
#38346=CARTESIAN_POINT('Origin',(16.1460502915689,-2.04566790084674,35.0294657090004));
#38347=CARTESIAN_POINT('',(8.05349305851944,42.8553320991532,33.8713886693271));
#38348=CARTESIAN_POINT('',(8.01409135636201,42.8553320991532,34.1916895598362));
#38349=CARTESIAN_POINT('Origin',(16.1460502915689,-2.04566790084674,35.0294657090004));
#38350=CARTESIAN_POINT('',(7.98602634532737,42.8553320991532,35.5240708007294));
#38351=CARTESIAN_POINT('',(7.97286324518834,42.8553320991532,35.2016240804971));
#38352=CARTESIAN_POINT('Origin',(16.1460502915689,23.3543320991532,35.0294657090004));
#38353=CARTESIAN_POINT('Origin',(16.1460502915689,-2.04566790084674,35.0294657090004));
#38354=CARTESIAN_POINT('',(7.98602634532736,42.8553320991532,34.5348606172715));
#38355=CARTESIAN_POINT('',(7.97286324518834,42.8553320991532,34.8573073375037));
#38356=CARTESIAN_POINT('Origin',(12.1460502915689,26.8543320991532,35.0294657090004));
#38357=CARTESIAN_POINT('Origin',(12.1460502915689,32.8543320991532,35.0294657090004));
#38358=CARTESIAN_POINT('Origin',(14.5360502915689,42.8543320991532,35.0294657090004));
#38359=CARTESIAN_POINT('Origin',(8.27105029156894,42.8553320991532,35.0294657090004));
#38360=CARTESIAN_POINT('',(8.27105029156894,42.8553320991532,35.0294657090004));
#38361=CARTESIAN_POINT('Origin',(8.27105029156894,42.8553320991532,35.0294657090004));
#38362=CARTESIAN_POINT('Origin',(8.29725370442717,42.8553320991532,35.6713513169335));
#38363=CARTESIAN_POINT('',(8.29725370442717,42.8553320991532,35.6713513169335));
#38364=CARTESIAN_POINT('Origin',(8.29725370442717,42.8553320991532,35.6713513169335));
#38365=CARTESIAN_POINT('Origin',(8.29725370442716,42.8553320991532,34.3875801010673));
#38366=CARTESIAN_POINT('',(8.29725370442716,42.8553320991532,34.3875801010673));
#38367=CARTESIAN_POINT('Origin',(8.29725370442716,42.8553320991532,34.3875801010673));
#38368=CARTESIAN_POINT('Origin',(8.37568956361252,42.8553320991532,33.7499661359513));
#38369=CARTESIAN_POINT('',(8.37568956361252,42.8553320991532,33.7499661359513));
#38370=CARTESIAN_POINT('Origin',(8.37568956361252,42.8553320991532,33.7499661359513));
#38371=CARTESIAN_POINT('Origin',(8.50583589142315,42.8553320991532,33.1208670293914));
#38372=CARTESIAN_POINT('',(8.50583589142315,42.8553320991532,33.1208670293914));
#38373=CARTESIAN_POINT('Origin',(8.50583589142315,42.8553320991532,33.1208670293914));
#38374=CARTESIAN_POINT('Origin',(8.68682658552011,42.8553320991532,32.5044693321477));
#38375=CARTESIAN_POINT('',(8.68682658552011,42.8553320991532,32.5044693321477));
#38376=CARTESIAN_POINT('Origin',(8.68682658552011,42.8553320991532,32.5044693321477));
#38377=CARTESIAN_POINT('Origin',(8.91745718269554,42.8553320991532,31.9048750691968));
#38378=CARTESIAN_POINT('',(8.91745718269554,42.8553320991532,31.9048750691968));
#38379=CARTESIAN_POINT('Origin',(8.91745718269554,42.8553320991532,31.9048750691968));
#38380=CARTESIAN_POINT('Origin',(9.19619287437661,42.8553320991532,31.3260744414326));
#38381=CARTESIAN_POINT('',(9.19619287437661,42.8553320991532,31.3260744414326));
#38382=CARTESIAN_POINT('Origin',(9.19619287437661,42.8553320991532,31.3260744414326));
#38383=CARTESIAN_POINT('Origin',(9.52117872052333,42.8553320991532,30.7719192715376));
#38384=CARTESIAN_POINT('',(9.52117872052333,42.8553320991532,30.7719192715376));
#38385=CARTESIAN_POINT('Origin',(9.52117872052333,42.8553320991532,30.7719192715376));
#38386=CARTESIAN_POINT('Origin',(9.89025199394849,42.8553320991532,30.2460973707382));
#38387=CARTESIAN_POINT('',(9.89025199394849,42.8553320991532,30.2460973707382));
#38388=CARTESIAN_POINT('Origin',(9.89025199394849,42.8553320991532,30.2460973707382));
#38389=CARTESIAN_POINT('Origin',(10.3009565729103,42.8553320991532,29.7521079970296));
#38390=CARTESIAN_POINT('',(10.3009565729103,42.8553320991532,29.7521079970296));
#38391=CARTESIAN_POINT('Origin',(10.3009565729103,42.8553320991532,29.7521079970296));
#38392=CARTESIAN_POINT('Origin',(10.7505592861971,42.8553320991532,29.2932385681916));
#38393=CARTESIAN_POINT('',(10.7505592861971,42.8553320991532,29.2932385681916));
#38394=CARTESIAN_POINT('Origin',(10.7505592861971,42.8553320991532,29.2932385681916));
#38395=CARTESIAN_POINT('Origin',(11.2360681019313,42.8553320991532,28.8725427845647));
#38396=CARTESIAN_POINT('',(11.2360681019313,42.8553320991532,28.8725427845647));
#38397=CARTESIAN_POINT('Origin',(11.2360681019313,42.8553320991532,28.8725427845647));
#38398=CARTESIAN_POINT('Origin',(11.7542520390476,42.8553320991532,28.4928203071792));
#38399=CARTESIAN_POINT('',(11.7542520390476,42.8553320991532,28.4928203071792));
#38400=CARTESIAN_POINT('Origin',(11.7542520390476,42.8553320991532,28.4928203071792));
#38401=CARTESIAN_POINT('Origin',(12.3016626689386,42.8553320991532,28.1565981264722));
#38402=CARTESIAN_POINT('',(12.3016626689386,42.8553320991532,28.1565981264722));
#38403=CARTESIAN_POINT('Origin',(12.3016626689386,42.8553320991532,28.1565981264722));
#38404=CARTESIAN_POINT('Origin',(12.874657064179,42.8553320991532,27.8661137455836));
#38405=CARTESIAN_POINT('',(12.874657064179,42.8553320991532,27.8661137455836));
#38406=CARTESIAN_POINT('Origin',(12.874657064179,42.8553320991532,27.8661137455836));
#38407=CARTESIAN_POINT('Origin',(13.4694220416057,42.8553320991532,27.6233002901416));
#38408=CARTESIAN_POINT('',(13.4694220416057,42.8553320991532,27.6233002901416));
#38409=CARTESIAN_POINT('Origin',(13.4694220416057,42.8553320991532,27.6233002901416));
#38410=CARTESIAN_POINT('Origin',(14.0819995384234,42.8553320991532,27.4297736436309));
#38411=CARTESIAN_POINT('',(14.0819995384234,42.8553320991532,27.4297736436309));
#38412=CARTESIAN_POINT('Origin',(14.0819995384234,42.8553320991532,27.4297736436309));
#38413=CARTESIAN_POINT('Origin',(14.7083129524589,42.8553320991532,27.2868216939543));
#38414=CARTESIAN_POINT('',(14.7083129524589,42.8553320991532,27.2868216939543));
#38415=CARTESIAN_POINT('Origin',(14.7083129524589,42.8553320991532,27.2868216939543));
#38416=CARTESIAN_POINT('Origin',(15.3441942712762,42.8553320991532,27.1953957627515));
#38417=CARTESIAN_POINT('',(15.3441942712762,42.8553320991532,27.1953957627515));
#38418=CARTESIAN_POINT('Origin',(15.3441942712762,42.8553320991532,27.1953957627515));
#38419=CARTESIAN_POINT('Origin',(15.9854118096115,42.8553320991532,27.1561042745104));
#38420=CARTESIAN_POINT('',(15.9854118096115,42.8553320991532,27.1561042745104));
#38421=CARTESIAN_POINT('Origin',(15.9854118096115,42.8553320991532,27.1561042745104));
#38422=CARTESIAN_POINT('Origin',(16.6276983705409,42.8553320991532,27.1692087076026));
#38423=CARTESIAN_POINT('',(16.6276983705409,42.8553320991532,27.1692087076026));
#38424=CARTESIAN_POINT('Origin',(16.6276983705409,42.8553320991532,27.1692087076026));
#38425=CARTESIAN_POINT('Origin',(17.266779642971,42.8553320991532,27.234621854188));
#38426=CARTESIAN_POINT('',(17.266779642971,42.8553320991532,27.234621854188));
#38427=CARTESIAN_POINT('Origin',(17.266779642971,42.8553320991532,27.234621854188));
#38428=CARTESIAN_POINT('Origin',(17.8984026464748,42.8553320991532,27.3519084005685));
#38429=CARTESIAN_POINT('',(17.8984026464748,42.8553320991532,27.3519084005685));
#38430=CARTESIAN_POINT('Origin',(17.8984026464748,42.8553320991532,27.3519084005685));
#38431=CARTESIAN_POINT('Origin',(18.5183640341746,42.8553320991532,27.5202878241288));
#38432=CARTESIAN_POINT('',(18.5183640341746,42.8553320991532,27.5202878241288));
#38433=CARTESIAN_POINT('Origin',(18.5183640341746,42.8553320991532,27.5202878241288));
#38434=CARTESIAN_POINT('Origin',(19.1225380653215,42.8553320991532,27.7386395875858));
#38435=CARTESIAN_POINT('',(19.1225380653215,42.8553320991532,27.7386395875858));
#38436=CARTESIAN_POINT('Origin',(19.1225380653215,42.8553320991532,27.7386395875858));
#38437=CARTESIAN_POINT('Origin',(19.70690406142,42.8553320991532,28.0055105959791));
#38438=CARTESIAN_POINT('',(19.70690406142,42.8553320991532,28.0055105959791));
#38439=CARTESIAN_POINT('Origin',(19.70690406142,42.8553320991532,28.0055105959791));
#38440=CARTESIAN_POINT('Origin',(20.2675731631797,42.8553320991532,28.3191248667786));
#38441=CARTESIAN_POINT('',(20.2675731631797,42.8553320991532,28.3191248667786));
#38442=CARTESIAN_POINT('Origin',(20.2675731631797,42.8553320991532,28.3191248667786));
#38443=CARTESIAN_POINT('Origin',(20.8008142102322,42.8553320991532,28.6773953487548));
#38444=CARTESIAN_POINT('',(20.8008142102322,42.8553320991532,28.6773953487548));
#38445=CARTESIAN_POINT('Origin',(20.8008142102322,42.8553320991532,28.6773953487548));
#38446=CARTESIAN_POINT('Origin',(21.303078571388,42.8553320991532,29.0779378109605));
#38447=CARTESIAN_POINT('',(21.303078571388,42.8553320991532,29.0779378109605));
#38448=CARTESIAN_POINT('Origin',(21.303078571388,42.8553320991532,29.0779378109605));
#38449=CARTESIAN_POINT('Origin',(21.7710237601914,42.8553320991532,29.5180867093948));
#38450=CARTESIAN_POINT('',(21.7710237601914,42.8553320991532,29.5180867093948));
#38451=CARTESIAN_POINT('Origin',(21.7710237601914,42.8553320991532,29.5180867093948));
#38452=CARTESIAN_POINT('Origin',(22.2015356786164,42.8553320991532,29.9949129257578));
#38453=CARTESIAN_POINT('',(22.2015356786164,42.8553320991532,29.9949129257578));
#38454=CARTESIAN_POINT('Origin',(22.2015356786164,42.8553320991532,29.9949129257578));
#38455=CARTESIAN_POINT('Origin',(22.5917493408753,42.8553320991532,30.5052432602507));
#38456=CARTESIAN_POINT('',(22.5917493408753,42.8553320991532,30.5052432602507));
#38457=CARTESIAN_POINT('Origin',(22.5917493408753,42.8553320991532,30.5052432602507));
#38458=CARTESIAN_POINT('Origin',(22.9390679394266,42.8553320991532,31.0456815486958));
#38459=CARTESIAN_POINT('',(22.9390679394266,42.8553320991532,31.0456815486958));
#38460=CARTESIAN_POINT('Origin',(22.9390679394266,42.8553320991532,31.0456815486958));
#38461=CARTESIAN_POINT('Origin',(23.2411801263005,42.8553320991532,31.6126312634495));
#38462=CARTESIAN_POINT('',(23.2411801263005,42.8553320991532,31.6126312634495));
#38463=CARTESIAN_POINT('Origin',(23.2411801263005,42.8553320991532,31.6126312634495));
#38464=CARTESIAN_POINT('Origin',(23.4960753947382,42.8553320991532,32.2023194477005));
#38465=CARTESIAN_POINT('',(23.4960753947382,42.8553320991532,32.2023194477005));
#38466=CARTESIAN_POINT('Origin',(23.4960753947382,42.8553320991532,32.2023194477005));
#38467=CARTESIAN_POINT('Origin',(23.7020574587831,42.8553320991532,32.8108218238741));
#38468=CARTESIAN_POINT('',(23.7020574587831,42.8553320991532,32.8108218238741));
#38469=CARTESIAN_POINT('Origin',(23.7020574587831,42.8553320991532,32.8108218238741));
#38470=CARTESIAN_POINT('Origin',(23.8577555417836,42.8553320991532,33.4340889090527));
#38471=CARTESIAN_POINT('',(23.8577555417836,42.8553320991532,33.4340889090527));
#38472=CARTESIAN_POINT('Origin',(23.8577555417836,42.8553320991532,33.4340889090527));
#38473=CARTESIAN_POINT('Origin',(23.9621334986858,42.8553320991532,34.0679729636163));
#38474=CARTESIAN_POINT('',(23.9621334986858,42.8553320991532,34.0679729636163));
#38475=CARTESIAN_POINT('Origin',(23.9621334986858,42.8553320991532,34.0679729636163));
#38476=CARTESIAN_POINT('Origin',(24.0144967114075,42.8553320991532,34.7082555937653));
#38477=CARTESIAN_POINT('',(24.0144967114075,42.8553320991532,34.7082555937653));
#38478=CARTESIAN_POINT('Origin',(24.0144967114075,42.8553320991532,34.7082555937653));
#38479=CARTESIAN_POINT('Origin',(24.0144967114075,42.8553320991532,35.3506758242353));
#38480=CARTESIAN_POINT('',(24.0144967114075,42.8553320991532,35.3506758242353));
#38481=CARTESIAN_POINT('Origin',(24.0144967114075,42.8553320991532,35.3506758242353));
#38482=CARTESIAN_POINT('Origin',(23.9621334986858,42.8553320991532,35.9909584543843));
#38483=CARTESIAN_POINT('',(23.9621334986858,42.8553320991532,35.9909584543843));
#38484=CARTESIAN_POINT('Origin',(23.9621334986858,42.8553320991532,35.9909584543843));
#38485=CARTESIAN_POINT('Origin',(23.8577555417836,42.8553320991532,36.6248425089479));
#38486=CARTESIAN_POINT('',(23.8577555417836,42.8553320991532,36.6248425089479));
#38487=CARTESIAN_POINT('Origin',(23.8577555417836,42.8553320991532,36.6248425089479));
#38488=CARTESIAN_POINT('Origin',(23.7020574587831,42.8553320991532,37.2481095941266));
#38489=CARTESIAN_POINT('',(23.7020574587831,42.8553320991532,37.2481095941266));
#38490=CARTESIAN_POINT('Origin',(23.7020574587831,42.8553320991532,37.2481095941266));
#38491=CARTESIAN_POINT('Origin',(23.4960753947382,42.8553320991532,37.8566119703002));
#38492=CARTESIAN_POINT('',(23.4960753947382,42.8553320991532,37.8566119703002));
#38493=CARTESIAN_POINT('Origin',(23.4960753947382,42.8553320991532,37.8566119703002));
#38494=CARTESIAN_POINT('Origin',(23.2411801263005,42.8553320991532,38.4463001545511));
#38495=CARTESIAN_POINT('',(23.2411801263005,42.8553320991532,38.4463001545511));
#38496=CARTESIAN_POINT('Origin',(23.2411801263005,42.8553320991532,38.4463001545511));
#38497=CARTESIAN_POINT('Origin',(22.9390679394267,42.8553320991532,39.0132498693049));
#38498=CARTESIAN_POINT('',(22.9390679394267,42.8553320991532,39.0132498693049));
#38499=CARTESIAN_POINT('Origin',(22.9390679394267,42.8553320991532,39.0132498693049));
#38500=CARTESIAN_POINT('Origin',(22.5917493408754,42.8553320991532,39.55368815775));
#38501=CARTESIAN_POINT('',(22.5917493408754,42.8553320991532,39.55368815775));
#38502=CARTESIAN_POINT('Origin',(22.5917493408754,42.8553320991532,39.55368815775));
#38503=CARTESIAN_POINT('Origin',(22.2015356786164,42.8553320991532,40.0640184922428));
#38504=CARTESIAN_POINT('',(22.2015356786164,42.8553320991532,40.0640184922428));
#38505=CARTESIAN_POINT('Origin',(22.2015356786164,42.8553320991532,40.0640184922428));
#38506=CARTESIAN_POINT('Origin',(21.7710237601915,42.8553320991532,40.5408447086059));
#38507=CARTESIAN_POINT('',(21.7710237601915,42.8553320991532,40.5408447086059));
#38508=CARTESIAN_POINT('Origin',(21.7710237601915,42.8553320991532,40.5408447086059));
#38509=CARTESIAN_POINT('Origin',(21.3030785713881,42.8553320991532,40.9809936070401));
#38510=CARTESIAN_POINT('',(21.3030785713881,42.8553320991532,40.9809936070401));
#38511=CARTESIAN_POINT('Origin',(21.3030785713881,42.8553320991532,40.9809936070401));
#38512=CARTESIAN_POINT('Origin',(20.8008142102323,42.8553320991532,41.3815360692459));
#38513=CARTESIAN_POINT('',(20.8008142102323,42.8553320991532,41.3815360692459));
#38514=CARTESIAN_POINT('Origin',(20.8008142102323,42.8553320991532,41.3815360692459));
#38515=CARTESIAN_POINT('Origin',(20.2675731631798,42.8553320991532,41.7398065512221));
#38516=CARTESIAN_POINT('',(20.2675731631798,42.8553320991532,41.7398065512221));
#38517=CARTESIAN_POINT('Origin',(20.2675731631798,42.8553320991532,41.7398065512221));
#38518=CARTESIAN_POINT('Origin',(19.7069040614201,42.8553320991532,42.0534208220216));
#38519=CARTESIAN_POINT('',(19.7069040614201,42.8553320991532,42.0534208220216));
#38520=CARTESIAN_POINT('Origin',(19.7069040614201,42.8553320991532,42.0534208220216));
#38521=CARTESIAN_POINT('Origin',(19.1225380653216,42.8553320991532,42.3202918304149));
#38522=CARTESIAN_POINT('',(19.1225380653216,42.8553320991532,42.3202918304149));
#38523=CARTESIAN_POINT('Origin',(19.1225380653216,42.8553320991532,42.3202918304149));
#38524=CARTESIAN_POINT('Origin',(18.5183640341747,42.8553320991532,42.5386435938719));
#38525=CARTESIAN_POINT('',(18.5183640341747,42.8553320991532,42.5386435938719));
#38526=CARTESIAN_POINT('Origin',(18.5183640341747,42.8553320991532,42.5386435938719));
#38527=CARTESIAN_POINT('Origin',(17.8984026464749,42.8553320991532,42.7070230174322));
#38528=CARTESIAN_POINT('',(17.8984026464749,42.8553320991532,42.7070230174322));
#38529=CARTESIAN_POINT('Origin',(17.8984026464749,42.8553320991532,42.7070230174322));
#38530=CARTESIAN_POINT('Origin',(17.2667796429711,42.8553320991532,42.8243095638127));
#38531=CARTESIAN_POINT('',(17.2667796429711,42.8553320991532,42.8243095638127));
#38532=CARTESIAN_POINT('Origin',(17.2667796429711,42.8553320991532,42.8243095638127));
#38533=CARTESIAN_POINT('Origin',(16.627698370541,42.8553320991532,42.8897227103981));
#38534=CARTESIAN_POINT('',(16.627698370541,42.8553320991532,42.8897227103981));
#38535=CARTESIAN_POINT('Origin',(16.627698370541,42.8553320991532,42.8897227103981));
#38536=CARTESIAN_POINT('Origin',(15.9854118096116,42.8553320991532,42.9028271434904));
#38537=CARTESIAN_POINT('',(15.9854118096116,42.8553320991532,42.9028271434904));
#38538=CARTESIAN_POINT('Origin',(15.9854118096116,42.8553320991532,42.9028271434904));
#38539=CARTESIAN_POINT('Origin',(15.3441942712763,42.8553320991532,42.8635356552493));
#38540=CARTESIAN_POINT('',(15.3441942712763,42.8553320991532,42.8635356552493));
#38541=CARTESIAN_POINT('Origin',(15.3441942712763,42.8553320991532,42.8635356552493));
#38542=CARTESIAN_POINT('Origin',(14.708312952459,42.8553320991532,42.7721097240465));
#38543=CARTESIAN_POINT('',(14.708312952459,42.8553320991532,42.7721097240465));
#38544=CARTESIAN_POINT('Origin',(14.708312952459,42.8553320991532,42.7721097240465));
#38545=CARTESIAN_POINT('Origin',(14.0819995384235,42.8553320991532,42.6291577743698));
#38546=CARTESIAN_POINT('',(14.0819995384235,42.8553320991532,42.6291577743698));
#38547=CARTESIAN_POINT('Origin',(14.0819995384235,42.8553320991532,42.6291577743698));
#38548=CARTESIAN_POINT('Origin',(13.4694220416058,42.8553320991532,42.4356311278591));
#38549=CARTESIAN_POINT('',(13.4694220416058,42.8553320991532,42.4356311278591));
#38550=CARTESIAN_POINT('Origin',(13.4694220416058,42.8553320991532,42.4356311278591));
#38551=CARTESIAN_POINT('Origin',(12.8746570641791,42.8553320991532,42.1928176724172));
#38552=CARTESIAN_POINT('',(12.8746570641791,42.8553320991532,42.1928176724172));
#38553=CARTESIAN_POINT('Origin',(12.8746570641791,42.8553320991532,42.1928176724172));
#38554=CARTESIAN_POINT('Origin',(12.3016626689387,42.8553320991532,41.9023332915286));
#38555=CARTESIAN_POINT('',(12.3016626689387,42.8553320991532,41.9023332915286));
#38556=CARTESIAN_POINT('Origin',(12.3016626689387,42.8553320991532,41.9023332915286));
#38557=CARTESIAN_POINT('Origin',(11.7542520390477,42.8553320991532,41.5661111108216));
#38558=CARTESIAN_POINT('',(11.7542520390477,42.8553320991532,41.5661111108216));
#38559=CARTESIAN_POINT('Origin',(11.7542520390477,42.8553320991532,41.5661111108216));
#38560=CARTESIAN_POINT('Origin',(11.2360681019314,42.8553320991532,41.1863886334361));
#38561=CARTESIAN_POINT('',(11.2360681019314,42.8553320991532,41.1863886334361));
#38562=CARTESIAN_POINT('Origin',(11.2360681019314,42.8553320991532,41.1863886334361));
#38563=CARTESIAN_POINT('Origin',(10.7505592861972,42.8553320991532,40.7656928498092));
#38564=CARTESIAN_POINT('',(10.7505592861972,42.8553320991532,40.7656928498092));
#38565=CARTESIAN_POINT('Origin',(10.7505592861972,42.8553320991532,40.7656928498092));
#38566=CARTESIAN_POINT('Origin',(10.3009565729103,42.8553320991532,40.3068234209711));
#38567=CARTESIAN_POINT('',(10.3009565729103,42.8553320991532,40.3068234209711));
#38568=CARTESIAN_POINT('Origin',(10.3009565729103,42.8553320991532,40.3068234209711));
#38569=CARTESIAN_POINT('Origin',(9.89025199394856,42.8553320991532,39.8128340472626));
#38570=CARTESIAN_POINT('',(9.89025199394856,42.8553320991532,39.8128340472626));
#38571=CARTESIAN_POINT('Origin',(9.89025199394856,42.8553320991532,39.8128340472626));
#38572=CARTESIAN_POINT('Origin',(9.52117872052339,42.8553320991532,39.2870121464632));
#38573=CARTESIAN_POINT('',(9.52117872052339,42.8553320991532,39.2870121464632));
#38574=CARTESIAN_POINT('Origin',(9.52117872052339,42.8553320991532,39.2870121464632));
#38575=CARTESIAN_POINT('Origin',(9.19619287437666,42.8553320991532,38.7328569765682));
#38576=CARTESIAN_POINT('',(9.19619287437666,42.8553320991532,38.7328569765682));
#38577=CARTESIAN_POINT('Origin',(9.19619287437666,42.8553320991532,38.7328569765682));
#38578=CARTESIAN_POINT('Origin',(8.91745718269558,42.8553320991532,38.154056348804));
#38579=CARTESIAN_POINT('',(8.91745718269558,42.8553320991532,38.154056348804));
#38580=CARTESIAN_POINT('Origin',(8.91745718269558,42.8553320991532,38.154056348804));
#38581=CARTESIAN_POINT('Origin',(8.68682658552015,42.8553320991532,37.5544620858532));
#38582=CARTESIAN_POINT('',(8.68682658552015,42.8553320991532,37.5544620858532));
#38583=CARTESIAN_POINT('Origin',(8.68682658552015,42.8553320991532,37.5544620858532));
#38584=CARTESIAN_POINT('Origin',(8.50583589142318,42.8553320991532,36.9380643886094));
#38585=CARTESIAN_POINT('',(8.50583589142318,42.8553320991532,36.9380643886094));
#38586=CARTESIAN_POINT('Origin',(8.50583589142318,42.8553320991532,36.9380643886094));
#38587=CARTESIAN_POINT('Origin',(8.37568956361254,42.8553320991532,36.3089652820495));
#38588=CARTESIAN_POINT('',(8.37568956361254,42.8553320991532,36.3089652820495));
#38589=CARTESIAN_POINT('Origin',(8.37568956361254,42.8553320991532,36.3089652820495));
#38590=CARTESIAN_POINT('',(34.1338186670738,3.31426102668157,32.1530708522187));
#38591=CARTESIAN_POINT('',(34.1338186670739,5.31426102668157,32.1530708522187));
#38592=CARTESIAN_POINT('',(34.1338186670738,17.3142610266922,32.1530708522187));
#38593=CARTESIAN_POINT('',(34.1338186670732,3.31426102668148,32.1530708522189));
#38594=CARTESIAN_POINT('',(34.1338186670738,3.31426102668157,32.1530708522187));
#38595=CARTESIAN_POINT('',(49.4990253396236,48.3142610266816,27.6909610474478));
#38596=CARTESIAN_POINT('',(34.1338186670377,76.7975758002401,32.1530708522828));
#38597=CARTESIAN_POINT('',(21.9999415741729,96.7519223609662,32.7724122825894));
#38598=CARTESIAN_POINT('',(-47.5389462217546,211.109687476565,36.3218395513712));
#38599=CARTESIAN_POINT('',(71.5729203425991,208.761409716205,-46.807935102884));
#38600=CARTESIAN_POINT('',(-34.6775982215323,218.514303809714,49.729202624551));
#38601=CARTESIAN_POINT('',(-23.1023850213318,225.178458509549,61.7958293904114));
#38602=CARTESIAN_POINT('',(-73.2616422222002,196.300454810265,9.50711340501639));
#38603=CARTESIAN_POINT('',(94.9654424283001,219.833323448903,-145.379669759802));
#38604=UNCERTAINTY_MEASURE_WITH_UNIT(LENGTH_MEASURE(0.01),#38636,
'DISTANCE_ACCURACY_VALUE',
'Maximum model space distance between geometric entities at asserted c
onnectivities');
#38605=UNCERTAINTY_MEASURE_WITH_UNIT(LENGTH_MEASURE(0.01),#38636,
'DISTANCE_ACCURACY_VALUE',
'Maximum model space distance between geometric entities at asserted c
onnectivities');
#38606=UNCERTAINTY_MEASURE_WITH_UNIT(LENGTH_MEASURE(0.01),#38636,
'DISTANCE_ACCURACY_VALUE',
'Maximum model space distance between geometric entities at asserted c
onnectivities');
#38607=UNCERTAINTY_MEASURE_WITH_UNIT(LENGTH_MEASURE(0.01),#38636,
'DISTANCE_ACCURACY_VALUE',
'Maximum model space distance between geometric entities at asserted c
onnectivities');
#38608=UNCERTAINTY_MEASURE_WITH_UNIT(LENGTH_MEASURE(0.01),#38636,
'DISTANCE_ACCURACY_VALUE',
'Maximum model space distance between geometric entities at asserted c
onnectivities');
#38609=UNCERTAINTY_MEASURE_WITH_UNIT(LENGTH_MEASURE(0.01),#38636,
'DISTANCE_ACCURACY_VALUE',
'Maximum model space distance between geometric entities at asserted c
onnectivities');
#38610=UNCERTAINTY_MEASURE_WITH_UNIT(LENGTH_MEASURE(0.01),#38636,
'DISTANCE_ACCURACY_VALUE',
'Maximum model space distance between geometric entities at asserted c
onnectivities');
#38611=UNCERTAINTY_MEASURE_WITH_UNIT(LENGTH_MEASURE(0.01),#38636,
'DISTANCE_ACCURACY_VALUE',
'Maximum model space distance between geometric entities at asserted c
onnectivities');
#38612=UNCERTAINTY_MEASURE_WITH_UNIT(LENGTH_MEASURE(0.01),#38636,
'DISTANCE_ACCURACY_VALUE',
'Maximum model space distance between geometric entities at asserted c
onnectivities');
#38613=UNCERTAINTY_MEASURE_WITH_UNIT(LENGTH_MEASURE(0.01),#38636,
'DISTANCE_ACCURACY_VALUE',
'Maximum model space distance between geometric entities at asserted c
onnectivities');
#38614=UNCERTAINTY_MEASURE_WITH_UNIT(LENGTH_MEASURE(0.01),#38636,
'DISTANCE_ACCURACY_VALUE',
'Maximum model space distance between geometric entities at asserted c
onnectivities');
#38615=UNCERTAINTY_MEASURE_WITH_UNIT(LENGTH_MEASURE(0.01),#38636,
'DISTANCE_ACCURACY_VALUE',
'Maximum model space distance between geometric entities at asserted c
onnectivities');
#38616=UNCERTAINTY_MEASURE_WITH_UNIT(LENGTH_MEASURE(0.01),#38636,
'DISTANCE_ACCURACY_VALUE',
'Maximum model space distance between geometric entities at asserted c
onnectivities');
#38617=UNCERTAINTY_MEASURE_WITH_UNIT(LENGTH_MEASURE(0.01),#38636,
'DISTANCE_ACCURACY_VALUE',
'Maximum model space distance between geometric entities at asserted c
onnectivities');
#38618=UNCERTAINTY_MEASURE_WITH_UNIT(LENGTH_MEASURE(0.01),#38636,
'DISTANCE_ACCURACY_VALUE',
'Maximum model space distance between geometric entities at asserted c
onnectivities');
#38619=UNCERTAINTY_MEASURE_WITH_UNIT(LENGTH_MEASURE(0.01),#38636,
'DISTANCE_ACCURACY_VALUE',
'Maximum model space distance between geometric entities at asserted c
onnectivities');
#38620=(
GEOMETRIC_REPRESENTATION_CONTEXT(3)
GLOBAL_UNCERTAINTY_ASSIGNED_CONTEXT((#38604))
GLOBAL_UNIT_ASSIGNED_CONTEXT((#38636,#38638,#38639))
REPRESENTATION_CONTEXT('','3D')
);
#38621=(
GEOMETRIC_REPRESENTATION_CONTEXT(3)
GLOBAL_UNCERTAINTY_ASSIGNED_CONTEXT((#38605))
GLOBAL_UNIT_ASSIGNED_CONTEXT((#38636,#38638,#38639))
REPRESENTATION_CONTEXT('','3D')
);
#38622=(
GEOMETRIC_REPRESENTATION_CONTEXT(3)
GLOBAL_UNCERTAINTY_ASSIGNED_CONTEXT((#38606))
GLOBAL_UNIT_ASSIGNED_CONTEXT((#38636,#38638,#38639))
REPRESENTATION_CONTEXT('','3D')
);
#38623=(
GEOMETRIC_REPRESENTATION_CONTEXT(3)
GLOBAL_UNCERTAINTY_ASSIGNED_CONTEXT((#38607))
GLOBAL_UNIT_ASSIGNED_CONTEXT((#38636,#38638,#38639))
REPRESENTATION_CONTEXT('','3D')
);
#38624=(
GEOMETRIC_REPRESENTATION_CONTEXT(3)
GLOBAL_UNCERTAINTY_ASSIGNED_CONTEXT((#38608))
GLOBAL_UNIT_ASSIGNED_CONTEXT((#38636,#38638,#38639))
REPRESENTATION_CONTEXT('','3D')
);
#38625=(
GEOMETRIC_REPRESENTATION_CONTEXT(3)
GLOBAL_UNCERTAINTY_ASSIGNED_CONTEXT((#38609))
GLOBAL_UNIT_ASSIGNED_CONTEXT((#38636,#38638,#38639))
REPRESENTATION_CONTEXT('','3D')
);
#38626=(
GEOMETRIC_REPRESENTATION_CONTEXT(3)
GLOBAL_UNCERTAINTY_ASSIGNED_CONTEXT((#38610))
GLOBAL_UNIT_ASSIGNED_CONTEXT((#38636,#38638,#38639))
REPRESENTATION_CONTEXT('','3D')
);
#38627=(
GEOMETRIC_REPRESENTATION_CONTEXT(3)
GLOBAL_UNCERTAINTY_ASSIGNED_CONTEXT((#38611))
GLOBAL_UNIT_ASSIGNED_CONTEXT((#38636,#38638,#38639))
REPRESENTATION_CONTEXT('','3D')
);
#38628=(
GEOMETRIC_REPRESENTATION_CONTEXT(3)
GLOBAL_UNCERTAINTY_ASSIGNED_CONTEXT((#38612))
GLOBAL_UNIT_ASSIGNED_CONTEXT((#38636,#38638,#38639))
REPRESENTATION_CONTEXT('','3D')
);
#38629=(
GEOMETRIC_REPRESENTATION_CONTEXT(3)
GLOBAL_UNCERTAINTY_ASSIGNED_CONTEXT((#38613))
GLOBAL_UNIT_ASSIGNED_CONTEXT((#38636,#38638,#38639))
REPRESENTATION_CONTEXT('','3D')
);
#38630=(
GEOMETRIC_REPRESENTATION_CONTEXT(3)
GLOBAL_UNCERTAINTY_ASSIGNED_CONTEXT((#38614))
GLOBAL_UNIT_ASSIGNED_CONTEXT((#38636,#38638,#38639))
REPRESENTATION_CONTEXT('','3D')
);
#38631=(
GEOMETRIC_REPRESENTATION_CONTEXT(3)
GLOBAL_UNCERTAINTY_ASSIGNED_CONTEXT((#38615))
GLOBAL_UNIT_ASSIGNED_CONTEXT((#38636,#38638,#38639))
REPRESENTATION_CONTEXT('','3D')
);
#38632=(
GEOMETRIC_REPRESENTATION_CONTEXT(3)
GLOBAL_UNCERTAINTY_ASSIGNED_CONTEXT((#38616))
GLOBAL_UNIT_ASSIGNED_CONTEXT((#38636,#38638,#38639))
REPRESENTATION_CONTEXT('','3D')
);
#38633=(
GEOMETRIC_REPRESENTATION_CONTEXT(3)
GLOBAL_UNCERTAINTY_ASSIGNED_CONTEXT((#38617))
GLOBAL_UNIT_ASSIGNED_CONTEXT((#38636,#38638,#38639))
REPRESENTATION_CONTEXT('','3D')
);
#38634=(
GEOMETRIC_REPRESENTATION_CONTEXT(3)
GLOBAL_UNCERTAINTY_ASSIGNED_CONTEXT((#38618))
GLOBAL_UNIT_ASSIGNED_CONTEXT((#38636,#38638,#38639))
REPRESENTATION_CONTEXT('','3D')
);
#38635=(
GEOMETRIC_REPRESENTATION_CONTEXT(3)
GLOBAL_UNCERTAINTY_ASSIGNED_CONTEXT((#38619))
GLOBAL_UNIT_ASSIGNED_CONTEXT((#38636,#38638,#38639))
REPRESENTATION_CONTEXT('','3D')
);
#38636=(
LENGTH_UNIT()
NAMED_UNIT(*)
SI_UNIT(.MILLI.,.METRE.)
);
#38637=(
LENGTH_UNIT()
NAMED_UNIT(*)
SI_UNIT($,.METRE.)
);
#38638=(
NAMED_UNIT(*)
PLANE_ANGLE_UNIT()
SI_UNIT($,.RADIAN.)
);
#38639=(
NAMED_UNIT(*)
SI_UNIT($,.STERADIAN.)
SOLID_ANGLE_UNIT()
);
#38640=SHAPE_DEFINITION_REPRESENTATION(#38655,#38684);
#38641=SHAPE_DEFINITION_REPRESENTATION(#38656,#38685);
#38642=SHAPE_DEFINITION_REPRESENTATION(#38657,#38686);
#38643=SHAPE_DEFINITION_REPRESENTATION(#38658,#38687);
#38644=SHAPE_DEFINITION_REPRESENTATION(#38659,#38688);
#38645=SHAPE_DEFINITION_REPRESENTATION(#38660,#38689);
#38646=SHAPE_DEFINITION_REPRESENTATION(#38661,#38690);
#38647=SHAPE_DEFINITION_REPRESENTATION(#38662,#38691);
#38648=SHAPE_DEFINITION_REPRESENTATION(#38663,#38692);
#38649=SHAPE_DEFINITION_REPRESENTATION(#38664,#38693);
#38650=SHAPE_DEFINITION_REPRESENTATION(#38665,#38694);
#38651=SHAPE_DEFINITION_REPRESENTATION(#38666,#38695);
#38652=SHAPE_DEFINITION_REPRESENTATION(#38667,#38696);
#38653=SHAPE_DEFINITION_REPRESENTATION(#38668,#38697);
#38654=SHAPE_DEFINITION_REPRESENTATION(#38669,#38698);
#38655=PRODUCT_DEFINITION_SHAPE('',$,#38700);
#38656=PRODUCT_DEFINITION_SHAPE('',$,#38701);
#38657=PRODUCT_DEFINITION_SHAPE('',$,#38702);
#38658=PRODUCT_DEFINITION_SHAPE('',$,#38703);
#38659=PRODUCT_DEFINITION_SHAPE('',$,#38704);
#38660=PRODUCT_DEFINITION_SHAPE('',$,#38705);
#38661=PRODUCT_DEFINITION_SHAPE('',$,#38706);
#38662=PRODUCT_DEFINITION_SHAPE('',$,#38707);
#38663=PRODUCT_DEFINITION_SHAPE('',$,#38708);
#38664=PRODUCT_DEFINITION_SHAPE('',$,#38709);
#38665=PRODUCT_DEFINITION_SHAPE('',$,#38710);
#38666=PRODUCT_DEFINITION_SHAPE('',$,#38711);
#38667=PRODUCT_DEFINITION_SHAPE('',$,#38712);
#38668=PRODUCT_DEFINITION_SHAPE('',$,#38713);
#38669=PRODUCT_DEFINITION_SHAPE('',$,#38714);
#38670=PRODUCT_DEFINITION_SHAPE($,$,#53);
#38671=PRODUCT_DEFINITION_SHAPE($,$,#54);
#38672=PRODUCT_DEFINITION_SHAPE($,$,#55);
#38673=PRODUCT_DEFINITION_SHAPE($,$,#56);
#38674=PRODUCT_DEFINITION_SHAPE($,$,#57);
#38675=PRODUCT_DEFINITION_SHAPE($,$,#58);
#38676=PRODUCT_DEFINITION_SHAPE($,$,#59);
#38677=PRODUCT_DEFINITION_SHAPE($,$,#60);
#38678=PRODUCT_DEFINITION_SHAPE($,$,#61);
#38679=PRODUCT_DEFINITION_SHAPE($,$,#62);
#38680=PRODUCT_DEFINITION_SHAPE($,$,#63);
#38681=PRODUCT_DEFINITION_SHAPE($,$,#64);
#38682=PRODUCT_DEFINITION_SHAPE($,$,#65);
#38683=PRODUCT_DEFINITION_SHAPE($,$,#66);
#38684=SHAPE_REPRESENTATION('',(#17787,#19729,#19730,#19731,#19732,#19733,
#19734,#19735,#19736,#19737,#19738,#19739,#19740,#19741,#19742),#38620);
#38685=SHAPE_REPRESENTATION('',(#17788),#38621);
#38686=SHAPE_REPRESENTATION('',(#17857),#38622);
#38687=SHAPE_REPRESENTATION('',(#17909),#38623);
#38688=SHAPE_REPRESENTATION('',(#18002),#38624);
#38689=SHAPE_REPRESENTATION('',(#18012),#38625);
#38690=SHAPE_REPRESENTATION('',(#18021),#38626);
#38691=SHAPE_REPRESENTATION('',(#18036),#38627);
#38692=SHAPE_REPRESENTATION('',(#18058),#38628);
#38693=SHAPE_REPRESENTATION('',(#18127),#38629);
#38694=SHAPE_REPRESENTATION('',(#18149),#38630);
#38695=SHAPE_REPRESENTATION('',(#18196),#38631);
#38696=SHAPE_REPRESENTATION('',(#18218),#38632);
#38697=SHAPE_REPRESENTATION('',(#18244),#38633);
#38698=SHAPE_REPRESENTATION('',(#18447),#38634);
#38699=PRODUCT_DEFINITION_CONTEXT('part definition',#38746,'design');
#38700=PRODUCT_DEFINITION('MAT-031','MAT-031',#38715,#38699);
#38701=PRODUCT_DEFINITION('Magnetic Base','Magnetic Base',#38716,#38699);
#38702=PRODUCT_DEFINITION('Magnetic Base Core','Magnetic Base Core',#38717,
#38699);
#38703=PRODUCT_DEFINITION('Base Cap','Base Cap',#38718,#38699);
#38704=PRODUCT_DEFINITION('Magnetic Base Bottom Cap',
'Magnetic Base Bottom Cap',#38719,#38699);
#38705=PRODUCT_DEFINITION('Magnetic Base Bottom Ring',
'Magnetic Base Bottom Ring',#38720,#38699);
#38706=PRODUCT_DEFINITION('Magnetic Base Switch','Magnetic Base Switch',
#38721,#38699);
#38707=PRODUCT_DEFINITION('Spherical Bearing','Spherical Bearing',#38722,
#38699);
#38708=PRODUCT_DEFINITION('Arm Joint 1','Arm Joint 1',#38723,#38699);
#38709=PRODUCT_DEFINITION('Arm Segment 1','Arm Segment 1',#38724,#38699);
#38710=PRODUCT_DEFINITION('Arm Joint 2','Arm Joint 2',#38725,#38699);
#38711=PRODUCT_DEFINITION('Arm Segment 2','Arm Segment 2',#38726,#38699);
#38712=PRODUCT_DEFINITION('Lock Screw','Lock Screw',#38727,#38699);
#38713=PRODUCT_DEFINITION('Star Knob','Star Knob',#38728,#38699);
#38714=PRODUCT_DEFINITION('Microfeed Holder','Microfeed Holder',#38729,
#38699);
#38715=PRODUCT_DEFINITION_FORMATION('',$,#38748);
#38716=PRODUCT_DEFINITION_FORMATION('',$,#38749);
#38717=PRODUCT_DEFINITION_FORMATION('',$,#38750);
#38718=PRODUCT_DEFINITION_FORMATION('',$,#38751);
#38719=PRODUCT_DEFINITION_FORMATION('',$,#38752);
#38720=PRODUCT_DEFINITION_FORMATION('',$,#38753);
#38721=PRODUCT_DEFINITION_FORMATION('',$,#38754);
#38722=PRODUCT_DEFINITION_FORMATION('',$,#38755);
#38723=PRODUCT_DEFINITION_FORMATION('',$,#38756);
#38724=PRODUCT_DEFINITION_FORMATION('',$,#38757);
#38725=PRODUCT_DEFINITION_FORMATION('',$,#38758);
#38726=PRODUCT_DEFINITION_FORMATION('',$,#38759);
#38727=PRODUCT_DEFINITION_FORMATION('',$,#38760);
#38728=PRODUCT_DEFINITION_FORMATION('',$,#38761);
#38729=PRODUCT_DEFINITION_FORMATION('',$,#38762);
#38730=PRODUCT_RELATED_PRODUCT_CATEGORY('MAT-031','MAT-031',(#38748));
#38731=PRODUCT_RELATED_PRODUCT_CATEGORY('Magnetic Base','Magnetic Base',
(#38749));
#38732=PRODUCT_RELATED_PRODUCT_CATEGORY('Magnetic Base Core',
'Magnetic Base Core',(#38750));
#38733=PRODUCT_RELATED_PRODUCT_CATEGORY('Base Cap','Base Cap',(#38751));
#38734=PRODUCT_RELATED_PRODUCT_CATEGORY('Magnetic Base Bottom Cap',
'Magnetic Base Bottom Cap',(#38752));
#38735=PRODUCT_RELATED_PRODUCT_CATEGORY('Magnetic Base Bottom Ring',
'Magnetic Base Bottom Ring',(#38753));
#38736=PRODUCT_RELATED_PRODUCT_CATEGORY('Magnetic Base Switch',
'Magnetic Base Switch',(#38754));
#38737=PRODUCT_RELATED_PRODUCT_CATEGORY('Spherical Bearing',
'Spherical Bearing',(#38755));
#38738=PRODUCT_RELATED_PRODUCT_CATEGORY('Arm Joint 1','Arm Joint 1',(#38756));
#38739=PRODUCT_RELATED_PRODUCT_CATEGORY('Arm Segment 1','Arm Segment 1',
(#38757));
#38740=PRODUCT_RELATED_PRODUCT_CATEGORY('Arm Joint 2','Arm Joint 2',(#38758));
#38741=PRODUCT_RELATED_PRODUCT_CATEGORY('Arm Segment 2','Arm Segment 2',
(#38759));
#38742=PRODUCT_RELATED_PRODUCT_CATEGORY('Lock Screw','Lock Screw',(#38760));
#38743=PRODUCT_RELATED_PRODUCT_CATEGORY('Star Knob','Star Knob',(#38761));
#38744=PRODUCT_RELATED_PRODUCT_CATEGORY('Microfeed Holder',
'Microfeed Holder',(#38762));
#38745=APPLICATION_PROTOCOL_DEFINITION('international standard',
'automotive_design',2009,#38746);
#38746=APPLICATION_CONTEXT(
'Core Data for Automotive Mechanical Design Process');
#38747=PRODUCT_CONTEXT('part definition',#38746,'mechanical');
#38748=PRODUCT('MAT-031','MAT-031','STEP AP214',(#38747));
#38749=PRODUCT('Magnetic Base','Magnetic Base',$,(#38747));
#38750=PRODUCT('Magnetic Base Core','Magnetic Base Core',$,(#38747));
#38751=PRODUCT('Base Cap','Base Cap',$,(#38747));
#38752=PRODUCT('Magnetic Base Bottom Cap','Magnetic Base Bottom Cap',$,
(#38747));
#38753=PRODUCT('Magnetic Base Bottom Ring','Magnetic Base Bottom Ring',
$,(#38747));
#38754=PRODUCT('Magnetic Base Switch','Magnetic Base Switch',$,(#38747));
#38755=PRODUCT('Spherical Bearing','Spherical Bearing',$,(#38747));
#38756=PRODUCT('Arm Joint 1','Arm Joint 1',$,(#38747));
#38757=PRODUCT('Arm Segment 1','Arm Segment 1',$,(#38747));
#38758=PRODUCT('Arm Joint 2','Arm Joint 2',$,(#38747));
#38759=PRODUCT('Arm Segment 2','Arm Segment 2',$,(#38747));
#38760=PRODUCT('Lock Screw','Lock Screw',$,(#38747));
#38761=PRODUCT('Star Knob','Star Knob',$,(#38747));
#38762=PRODUCT('Microfeed Holder','Microfeed Holder',$,(#38747));
#38763=PRESENTATION_STYLE_ASSIGNMENT((#38770));
#38764=PRESENTATION_STYLE_ASSIGNMENT((#38771));
#38765=PRESENTATION_STYLE_ASSIGNMENT((#38772));
#38766=PRESENTATION_STYLE_ASSIGNMENT((#38773));
#38767=PRESENTATION_STYLE_ASSIGNMENT((#38774));
#38768=PRESENTATION_STYLE_ASSIGNMENT((#38775));
#38769=PRESENTATION_STYLE_ASSIGNMENT((#38776));
#38770=SURFACE_STYLE_USAGE(.BOTH.,#38777);
#38771=SURFACE_STYLE_USAGE(.BOTH.,#38778);
#38772=SURFACE_STYLE_USAGE(.BOTH.,#38779);
#38773=SURFACE_STYLE_USAGE(.BOTH.,#38780);
#38774=SURFACE_STYLE_USAGE(.BOTH.,#38781);
#38775=SURFACE_STYLE_USAGE(.BOTH.,#38782);
#38776=SURFACE_STYLE_USAGE(.BOTH.,#38783);
#38777=SURFACE_SIDE_STYLE('',(#38784));
#38778=SURFACE_SIDE_STYLE('',(#38785));
#38779=SURFACE_SIDE_STYLE('',(#38786));
#38780=SURFACE_SIDE_STYLE('',(#38787));
#38781=SURFACE_SIDE_STYLE('',(#38788));
#38782=SURFACE_SIDE_STYLE('',(#38789));
#38783=SURFACE_SIDE_STYLE('',(#38790));
#38784=SURFACE_STYLE_FILL_AREA(#38791);
#38785=SURFACE_STYLE_FILL_AREA(#38792);
#38786=SURFACE_STYLE_FILL_AREA(#38793);
#38787=SURFACE_STYLE_FILL_AREA(#38794);
#38788=SURFACE_STYLE_FILL_AREA(#38795);
#38789=SURFACE_STYLE_FILL_AREA(#38796);
#38790=SURFACE_STYLE_FILL_AREA(#38797);
#38791=FILL_AREA_STYLE('Steel - Satin',(#38798));
#38792=FILL_AREA_STYLE('Opaque(20,51,87)',(#38799));
#38793=FILL_AREA_STYLE('Opaque(227,224,212)',(#38800));
#38794=FILL_AREA_STYLE('Opaque(61,176,222)',(#38801));
#38795=FILL_AREA_STYLE('Opaque(97,158,199)',(#38802));
#38796=FILL_AREA_STYLE('Opaque(122,133,145)',(#38803));
#38797=FILL_AREA_STYLE('Opaque(31,36,43)',(#38804));
#38798=FILL_AREA_STYLE_COLOUR('Steel - Satin',#38805);
#38799=FILL_AREA_STYLE_COLOUR('Opaque(20,51,87)',#38806);
#38800=FILL_AREA_STYLE_COLOUR('Opaque(227,224,212)',#38807);
#38801=FILL_AREA_STYLE_COLOUR('Opaque(61,176,222)',#38808);
#38802=FILL_AREA_STYLE_COLOUR('Opaque(97,158,199)',#38809);
#38803=FILL_AREA_STYLE_COLOUR('Opaque(122,133,145)',#38810);
#38804=FILL_AREA_STYLE_COLOUR('Opaque(31,36,43)',#38811);
#38805=COLOUR_RGB('Steel - Satin',0.627450980392157,0.627450980392157,0.627450980392157);
#38806=COLOUR_RGB('Opaque(20,51,87)',0.0784313725490196,0.2,0.341176470588235);
#38807=COLOUR_RGB('Opaque(227,224,212)',0.890196078431372,0.87843137254902,
0.831372549019608);
#38808=COLOUR_RGB('Opaque(61,176,222)',0.23921568627451,0.690196078431373,
0.870588235294118);
#38809=COLOUR_RGB('Opaque(97,158,199)',0.380392156862745,0.619607843137255,
0.780392156862745);
#38810=COLOUR_RGB('Opaque(122,133,145)',0.47843137254902,0.52156862745098,
0.568627450980392);
#38811=COLOUR_RGB('Opaque(31,36,43)',0.12156862745098,0.141176470588235,
0.168627450980392);
ENDSEC;
END-ISO-10303-21;
